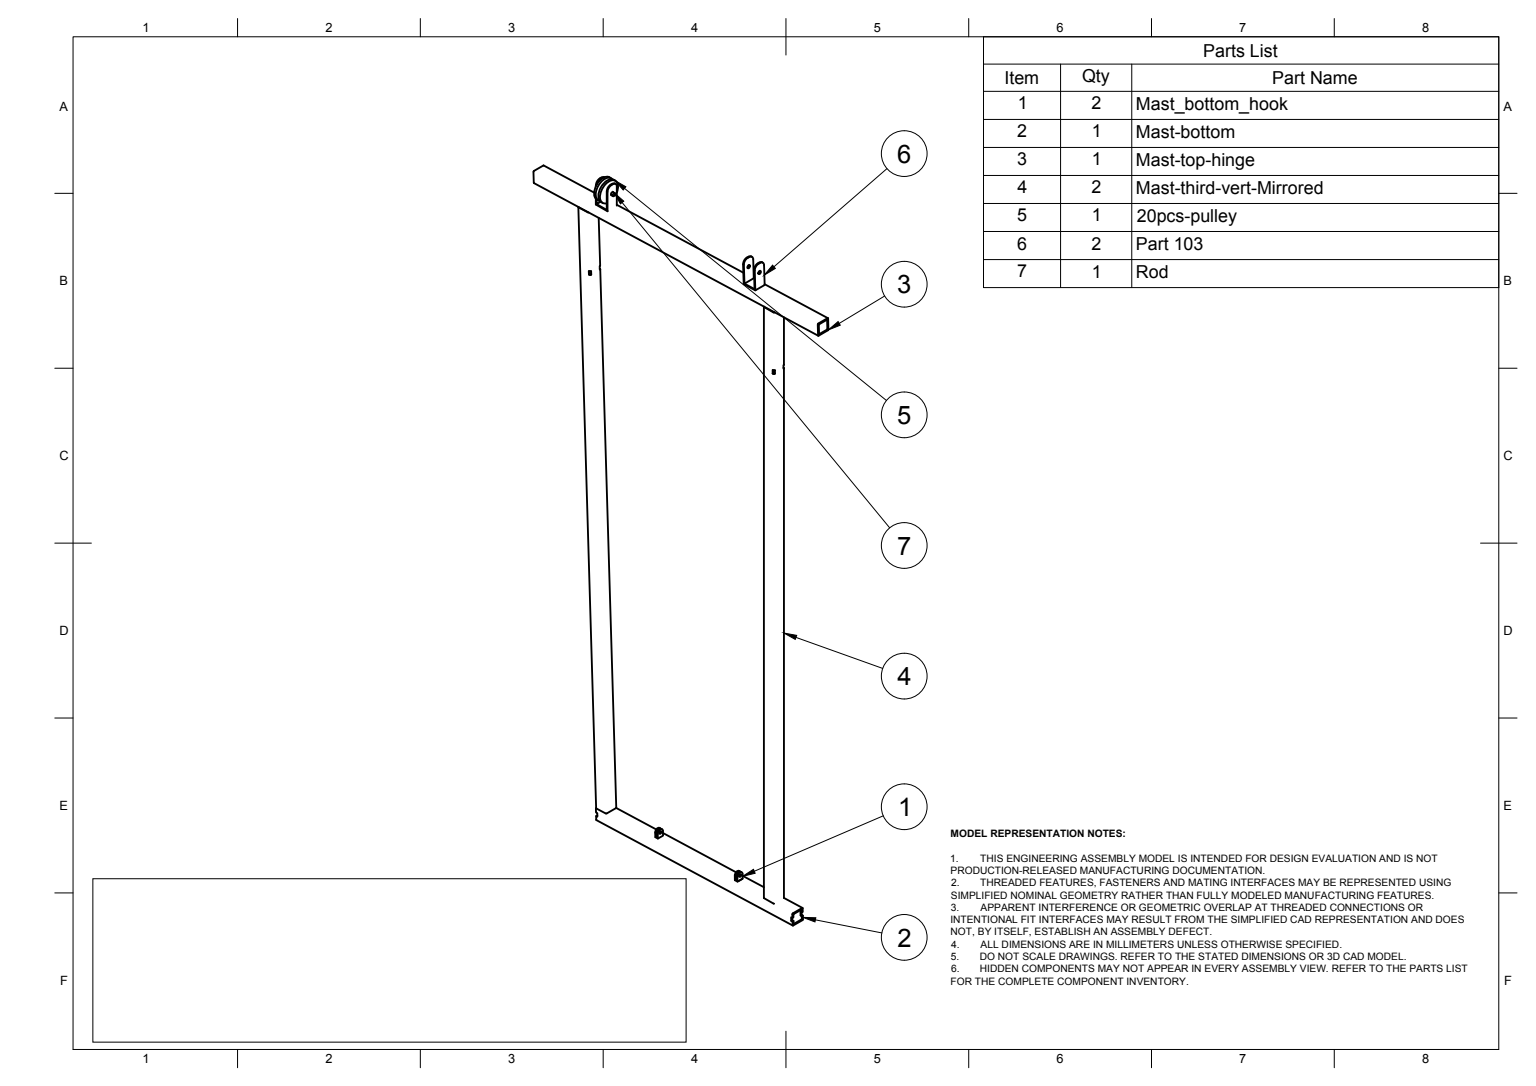
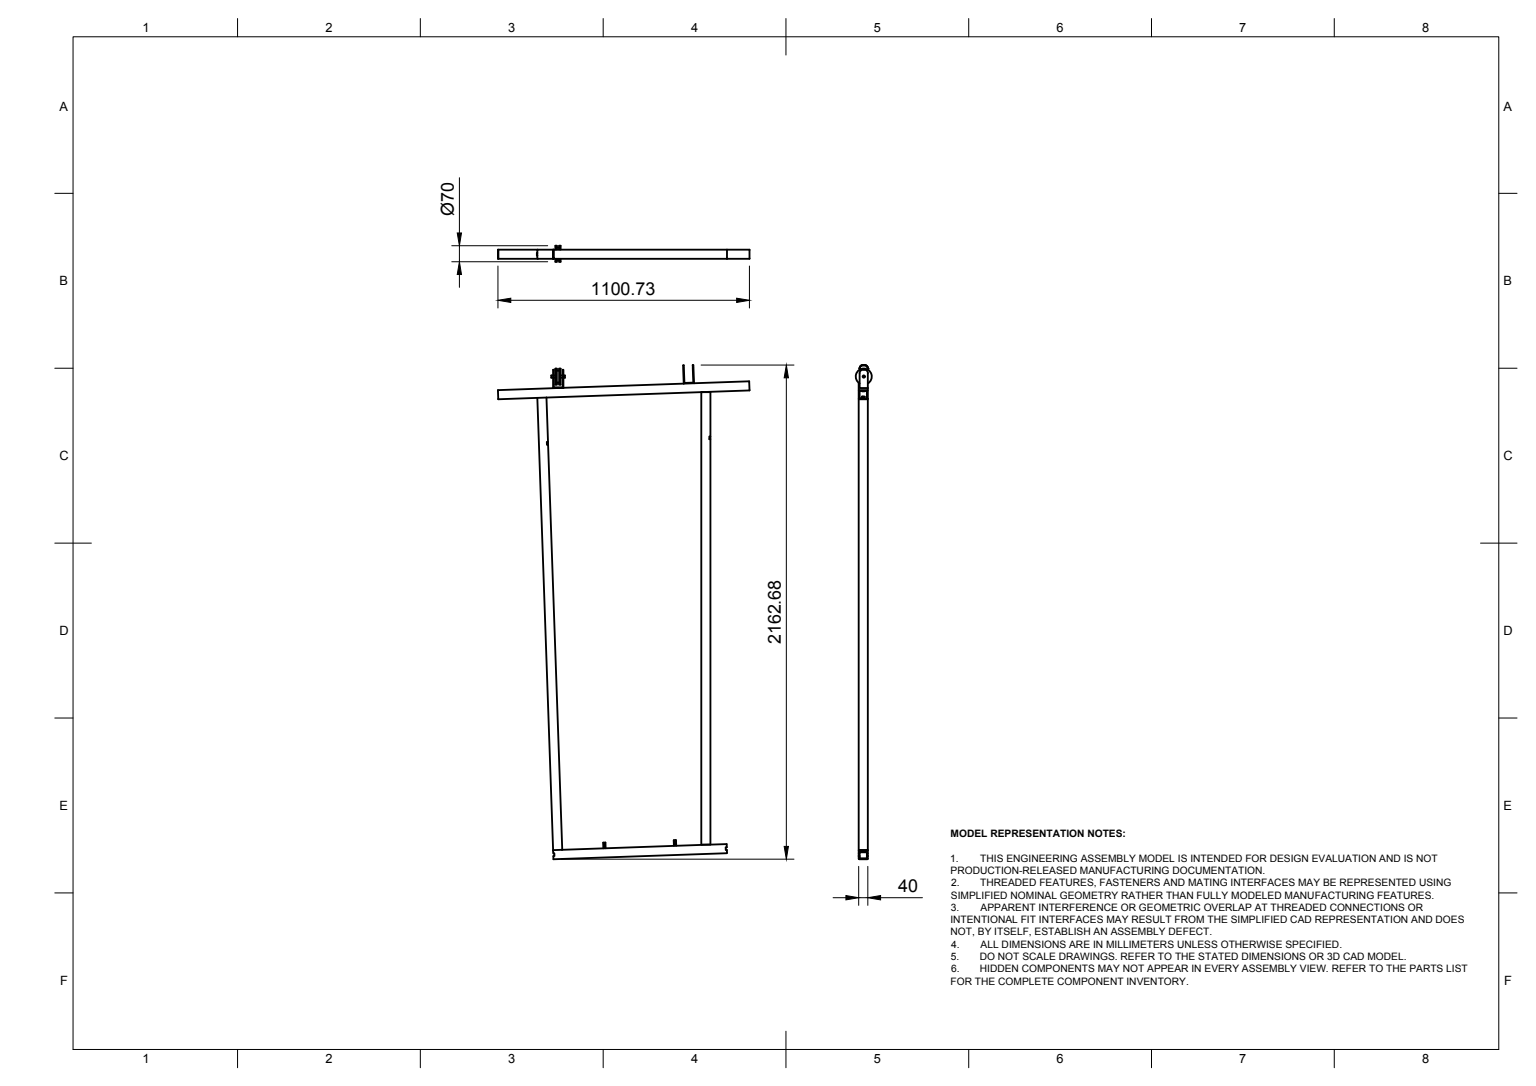
ISO-10303-21;
HEADER;
/* Generated by software containing ST-Developer
 * from STEP Tools, Inc. (www.steptools.com) 
 */

FILE_DESCRIPTION(
/* description */ (''),
/* implementation_level */ '2;1');

FILE_NAME(
/* name */ 'MAS-605',
/* time_stamp */ '2026-10-07T11:02:43-07:00',
/* author */ (''),
/* organization */ (''),
/* preprocessor_version */ 'ST-DEVELOPER v20.2',
/* originating_system */ 'Autodesk Translation Framework v15.15.0.0',
/* authorisation */ '');

FILE_SCHEMA (('AUTOMOTIVE_DESIGN { 1 0 10303 214 3 1 1 }'));
ENDSEC;

DATA;
#10=MECHANICAL_DESIGN_GEOMETRIC_PRESENTATION_REPRESENTATION('',(#66,#67,
#68,#69,#70,#71,#72),#5505);
#11=ITEM_DEFINED_TRANSFORMATION($,$,#3575,#3635);
#12=ITEM_DEFINED_TRANSFORMATION($,$,#3379,#3636);
#13=ITEM_DEFINED_TRANSFORMATION($,$,#3436,#3637);
#14=ITEM_DEFINED_TRANSFORMATION($,$,#3519,#3638);
#15=ITEM_DEFINED_TRANSFORMATION($,$,#3495,#3639);
#16=ITEM_DEFINED_TRANSFORMATION($,$,#3601,#3640);
#17=ITEM_DEFINED_TRANSFORMATION($,$,#3513,#3641);
#18=ITEM_DEFINED_TRANSFORMATION($,$,#3519,#3642);
#19=ITEM_DEFINED_TRANSFORMATION($,$,#3575,#3643);
#20=ITEM_DEFINED_TRANSFORMATION($,$,#3601,#3644);
#21=(
REPRESENTATION_RELATIONSHIP($,$,#5542,#5536)
REPRESENTATION_RELATIONSHIP_WITH_TRANSFORMATION(#11)
SHAPE_REPRESENTATION_RELATIONSHIP()
);
#22=(
REPRESENTATION_RELATIONSHIP($,$,#5537,#5536)
REPRESENTATION_RELATIONSHIP_WITH_TRANSFORMATION(#12)
SHAPE_REPRESENTATION_RELATIONSHIP()
);
#23=(
REPRESENTATION_RELATIONSHIP($,$,#5538,#5536)
REPRESENTATION_RELATIONSHIP_WITH_TRANSFORMATION(#13)
SHAPE_REPRESENTATION_RELATIONSHIP()
);
#24=(
REPRESENTATION_RELATIONSHIP($,$,#5541,#5536)
REPRESENTATION_RELATIONSHIP_WITH_TRANSFORMATION(#14)
SHAPE_REPRESENTATION_RELATIONSHIP()
);
#25=(
REPRESENTATION_RELATIONSHIP($,$,#5539,#5536)
REPRESENTATION_RELATIONSHIP_WITH_TRANSFORMATION(#15)
SHAPE_REPRESENTATION_RELATIONSHIP()
);
#26=(
REPRESENTATION_RELATIONSHIP($,$,#5543,#5536)
REPRESENTATION_RELATIONSHIP_WITH_TRANSFORMATION(#16)
SHAPE_REPRESENTATION_RELATIONSHIP()
);
#27=(
REPRESENTATION_RELATIONSHIP($,$,#5540,#5536)
REPRESENTATION_RELATIONSHIP_WITH_TRANSFORMATION(#17)
SHAPE_REPRESENTATION_RELATIONSHIP()
);
#28=(
REPRESENTATION_RELATIONSHIP($,$,#5541,#5536)
REPRESENTATION_RELATIONSHIP_WITH_TRANSFORMATION(#18)
SHAPE_REPRESENTATION_RELATIONSHIP()
);
#29=(
REPRESENTATION_RELATIONSHIP($,$,#5542,#5536)
REPRESENTATION_RELATIONSHIP_WITH_TRANSFORMATION(#19)
SHAPE_REPRESENTATION_RELATIONSHIP()
);
#30=(
REPRESENTATION_RELATIONSHIP($,$,#5543,#5536)
REPRESENTATION_RELATIONSHIP_WITH_TRANSFORMATION(#20)
SHAPE_REPRESENTATION_RELATIONSHIP()
);
#31=CONTEXT_DEPENDENT_SHAPE_REPRESENTATION(#21,#5526);
#32=CONTEXT_DEPENDENT_SHAPE_REPRESENTATION(#22,#5527);
#33=CONTEXT_DEPENDENT_SHAPE_REPRESENTATION(#23,#5528);
#34=CONTEXT_DEPENDENT_SHAPE_REPRESENTATION(#24,#5529);
#35=CONTEXT_DEPENDENT_SHAPE_REPRESENTATION(#25,#5530);
#36=CONTEXT_DEPENDENT_SHAPE_REPRESENTATION(#26,#5531);
#37=CONTEXT_DEPENDENT_SHAPE_REPRESENTATION(#27,#5532);
#38=CONTEXT_DEPENDENT_SHAPE_REPRESENTATION(#28,#5533);
#39=CONTEXT_DEPENDENT_SHAPE_REPRESENTATION(#29,#5534);
#40=CONTEXT_DEPENDENT_SHAPE_REPRESENTATION(#30,#5535);
#41=NEXT_ASSEMBLY_USAGE_OCCURRENCE('Mast_bottom_hook:1',
'Mast_bottom_hook:1','Mast_bottom_hook:1',#5545,#5551,
'Mast_bottom_hook:1');
#42=NEXT_ASSEMBLY_USAGE_OCCURRENCE('Mast-bottom:1','Mast-bottom:1',
'Mast-bottom:1',#5545,#5546,'Mast-bottom:1');
#43=NEXT_ASSEMBLY_USAGE_OCCURRENCE('Mast-top-hinge:1',
'Mast-top-hinge:1','Mast-top-hinge:1',#5545,#5547,'Mast-top-hinge:1');
#44=NEXT_ASSEMBLY_USAGE_OCCURRENCE('Mast-third-vert-Mirrored:1',
'Mast-third-vert-Mirrored:1','Mast-third-vert-Mirrored:1',#5545,#5550,
'Mast-third-vert-Mirrored:1');
#45=NEXT_ASSEMBLY_USAGE_OCCURRENCE('Pulley:1','Pulley:1','Pulley:1',#5545,
#5548,'Pulley:1');
#46=NEXT_ASSEMBLY_USAGE_OCCURRENCE('Part 103:1','Part 103:1',
'Part 103:1',#5545,#5552,'Part 103:1');
#47=NEXT_ASSEMBLY_USAGE_OCCURRENCE('rod:1','rod:1','rod:1',#5545,#5549,
'rod:1');
#48=NEXT_ASSEMBLY_USAGE_OCCURRENCE('Mast-third-vert-Mirrored:2',
'Mast-third-vert-Mirrored:2','Mast-third-vert-Mirrored:2',#5545,#5550,
'Mast-third-vert-Mirrored:2');
#49=NEXT_ASSEMBLY_USAGE_OCCURRENCE('Mast_bottom_hook:2',
'Mast_bottom_hook:2','Mast_bottom_hook:2',#5545,#5551,
'Mast_bottom_hook:2');
#50=NEXT_ASSEMBLY_USAGE_OCCURRENCE('Part 103:2','Part 103:2',
'Part 103:2',#5545,#5552,'Part 103:2');
#51=TOROIDAL_SURFACE('',#3505,30.,5.);
#52=SHAPE_REPRESENTATION_RELATIONSHIP('SRR','None',#5537,#59);
#53=SHAPE_REPRESENTATION_RELATIONSHIP('SRR','None',#5538,#60);
#54=SHAPE_REPRESENTATION_RELATIONSHIP('SRR','None',#5539,#61);
#55=SHAPE_REPRESENTATION_RELATIONSHIP('SRR','None',#5540,#62);
#56=SHAPE_REPRESENTATION_RELATIONSHIP('SRR','None',#5541,#63);
#57=SHAPE_REPRESENTATION_RELATIONSHIP('SRR','None',#5542,#64);
#58=SHAPE_REPRESENTATION_RELATIONSHIP('SRR','None',#5543,#65);
#59=ADVANCED_BREP_SHAPE_REPRESENTATION('',(#73),#5498);
#60=ADVANCED_BREP_SHAPE_REPRESENTATION('',(#74),#5499);
#61=ADVANCED_BREP_SHAPE_REPRESENTATION('',(#75),#5500);
#62=ADVANCED_BREP_SHAPE_REPRESENTATION('',(#76),#5501);
#63=ADVANCED_BREP_SHAPE_REPRESENTATION('',(#77),#5502);
#64=ADVANCED_BREP_SHAPE_REPRESENTATION('',(#78),#5503);
#65=ADVANCED_BREP_SHAPE_REPRESENTATION('',(#79),#5504);
#66=STYLED_ITEM('',(#5581),#73);
#67=STYLED_ITEM('',(#5582),#74);
#68=STYLED_ITEM('',(#5583),#75);
#69=STYLED_ITEM('',(#5584),#76);
#70=STYLED_ITEM('',(#5585),#77);
#71=STYLED_ITEM('',(#5586),#78);
#72=STYLED_ITEM('',(#5587),#79);
#73=MANIFOLD_SOLID_BREP('Body1',#3293);
#74=MANIFOLD_SOLID_BREP('Body1',#3294);
#75=MANIFOLD_SOLID_BREP('Body1',#3295);
#76=MANIFOLD_SOLID_BREP('Body1',#3296);
#77=MANIFOLD_SOLID_BREP('Body1',#3297);
#78=MANIFOLD_SOLID_BREP('Body1',#3298);
#79=MANIFOLD_SOLID_BREP('Body1',#3299);
#80=FACE_BOUND('',#416,.T.);
#81=FACE_BOUND('',#417,.T.);
#82=FACE_BOUND('',#428,.T.);
#83=FACE_BOUND('',#429,.T.);
#84=FACE_BOUND('',#447,.T.);
#85=FACE_BOUND('',#448,.T.);
#86=FACE_BOUND('',#450,.T.);
#87=FACE_BOUND('',#451,.T.);
#88=FACE_BOUND('',#461,.T.);
#89=FACE_BOUND('',#462,.T.);
#90=FACE_BOUND('',#463,.T.);
#91=FACE_BOUND('',#464,.T.);
#92=FACE_BOUND('',#466,.T.);
#93=FACE_BOUND('',#467,.T.);
#94=FACE_BOUND('',#468,.T.);
#95=FACE_BOUND('',#469,.T.);
#96=FACE_BOUND('',#477,.T.);
#97=FACE_BOUND('',#479,.T.);
#98=FACE_BOUND('',#504,.T.);
#99=FACE_BOUND('',#507,.T.);
#100=FACE_BOUND('',#510,.T.);
#101=FACE_BOUND('',#513,.T.);
#102=FACE_BOUND('',#532,.T.);
#103=FACE_BOUND('',#554,.T.);
#104=FACE_BOUND('',#556,.T.);
#105=FACE_BOUND('',#558,.T.);
#106=FACE_BOUND('',#560,.T.);
#107=FACE_BOUND('',#562,.T.);
#108=FACE_BOUND('',#577,.T.);
#109=FACE_BOUND('',#579,.T.);
#110=FACE_BOUND('',#582,.T.);
#111=FACE_BOUND('',#584,.T.);
#112=FACE_BOUND('',#586,.T.);
#113=CYLINDRICAL_SURFACE('',#3399,2.);
#114=CYLINDRICAL_SURFACE('',#3401,2.);
#115=CYLINDRICAL_SURFACE('',#3404,2.);
#116=CYLINDRICAL_SURFACE('',#3406,2.);
#117=CYLINDRICAL_SURFACE('',#3414,1.8);
#118=CYLINDRICAL_SURFACE('',#3415,1.8);
#119=CYLINDRICAL_SURFACE('',#3417,1.8);
#120=CYLINDRICAL_SURFACE('',#3418,1.8);
#121=CYLINDRICAL_SURFACE('',#3450,2.);
#122=CYLINDRICAL_SURFACE('',#3453,2.);
#123=CYLINDRICAL_SURFACE('',#3457,2.);
#124=CYLINDRICAL_SURFACE('',#3460,2.);
#125=CYLINDRICAL_SURFACE('',#3473,1.8);
#126=CYLINDRICAL_SURFACE('',#3474,1.8);
#127=CYLINDRICAL_SURFACE('',#3476,1.8);
#128=CYLINDRICAL_SURFACE('',#3477,1.8);
#129=CYLINDRICAL_SURFACE('',#3496,5.);
#130=CYLINDRICAL_SURFACE('',#3501,35.);
#131=CYLINDRICAL_SURFACE('',#3510,35.);
#132=CYLINDRICAL_SURFACE('',#3516,5.);
#133=CYLINDRICAL_SURFACE('',#3531,2.);
#134=CYLINDRICAL_SURFACE('',#3535,2.);
#135=CYLINDRICAL_SURFACE('',#3538,1.8);
#136=CYLINDRICAL_SURFACE('',#3541,1.8);
#137=CYLINDRICAL_SURFACE('',#3544,1.8);
#138=CYLINDRICAL_SURFACE('',#3547,1.8);
#139=CYLINDRICAL_SURFACE('',#3553,2.);
#140=CYLINDRICAL_SURFACE('',#3556,2.);
#141=CYLINDRICAL_SURFACE('',#3558,2.);
#142=CYLINDRICAL_SURFACE('',#3559,2.);
#143=CYLINDRICAL_SURFACE('',#3592,4.);
#144=CYLINDRICAL_SURFACE('',#3593,4.);
#145=CYLINDRICAL_SURFACE('',#3594,10.);
#146=CYLINDRICAL_SURFACE('',#3595,10.);
#147=CYLINDRICAL_SURFACE('',#3629,15.);
#148=CYLINDRICAL_SURFACE('',#3630,15.);
#149=CYLINDRICAL_SURFACE('',#3631,15.);
#150=CYLINDRICAL_SURFACE('',#3632,15.);
#151=CYLINDRICAL_SURFACE('',#3633,5.);
#152=CYLINDRICAL_SURFACE('',#3634,5.);
#153=CIRCLE('',#3385,1.8);
#154=CIRCLE('',#3386,1.8);
#155=CIRCLE('',#3387,2.);
#156=CIRCLE('',#3388,2.);
#157=CIRCLE('',#3392,2.);
#158=CIRCLE('',#3393,2.);
#159=CIRCLE('',#3394,1.8);
#160=CIRCLE('',#3395,1.8);
#161=CIRCLE('',#3400,2.);
#162=CIRCLE('',#3402,2.);
#163=CIRCLE('',#3405,2.);
#164=CIRCLE('',#3407,2.);
#165=CIRCLE('',#3409,1.8);
#166=CIRCLE('',#3410,1.8);
#167=CIRCLE('',#3412,1.8);
#168=CIRCLE('',#3413,1.8);
#169=CIRCLE('',#3451,2.);
#170=CIRCLE('',#3452,2.);
#171=CIRCLE('',#3454,2.);
#172=CIRCLE('',#3455,2.);
#173=CIRCLE('',#3458,2.);
#174=CIRCLE('',#3459,2.);
#175=CIRCLE('',#3461,2.);
#176=CIRCLE('',#3462,2.);
#177=CIRCLE('',#3464,1.8);
#178=CIRCLE('',#3465,1.8);
#179=CIRCLE('',#3466,1.8);
#180=CIRCLE('',#3467,1.8);
#181=CIRCLE('',#3469,1.8);
#182=CIRCLE('',#3470,1.8);
#183=CIRCLE('',#3471,1.8);
#184=CIRCLE('',#3472,1.8);
#185=CIRCLE('',#3497,5.);
#186=CIRCLE('',#3498,5.);
#187=CIRCLE('',#3500,35.);
#188=CIRCLE('',#3502,35.);
#189=CIRCLE('',#3504,30.);
#190=CIRCLE('',#3506,5.);
#191=CIRCLE('',#3507,30.);
#192=CIRCLE('',#3509,35.);
#193=CIRCLE('',#3511,35.);
#194=CIRCLE('',#3515,5.);
#195=CIRCLE('',#3517,5.);
#196=CIRCLE('',#3521,1.8);
#197=CIRCLE('',#3522,1.8);
#198=CIRCLE('',#3523,2.);
#199=CIRCLE('',#3524,2.);
#200=CIRCLE('',#3526,2.);
#201=CIRCLE('',#3527,2.);
#202=CIRCLE('',#3528,1.8);
#203=CIRCLE('',#3529,1.8);
#204=CIRCLE('',#3532,2.);
#205=CIRCLE('',#3533,2.);
#206=CIRCLE('',#3536,2.);
#207=CIRCLE('',#3539,1.8);
#208=CIRCLE('',#3542,1.8);
#209=CIRCLE('',#3545,1.8);
#210=CIRCLE('',#3548,1.8);
#211=CIRCLE('',#3550,2.);
#212=CIRCLE('',#3551,2.);
#213=CIRCLE('',#3552,2.);
#214=CIRCLE('',#3554,2.);
#215=CIRCLE('',#3560,2.);
#216=CIRCLE('',#3578,10.);
#217=CIRCLE('',#3579,4.);
#218=CIRCLE('',#3581,10.);
#219=CIRCLE('',#3582,4.);
#220=CIRCLE('',#3584,10.);
#221=CIRCLE('',#3585,4.);
#222=CIRCLE('',#3587,10.);
#223=CIRCLE('',#3588,4.);
#224=CIRCLE('',#3604,15.);
#225=CIRCLE('',#3605,15.);
#226=CIRCLE('',#3606,5.);
#227=CIRCLE('',#3608,15.);
#228=CIRCLE('',#3609,15.);
#229=CIRCLE('',#3610,5.);
#230=CIRCLE('',#3613,15.);
#231=CIRCLE('',#3614,15.);
#232=CIRCLE('',#3615,5.);
#233=CIRCLE('',#3617,15.);
#234=CIRCLE('',#3618,15.);
#235=CIRCLE('',#3619,5.);
#236=FACE_OUTER_BOUND('',#402,.T.);
#237=FACE_OUTER_BOUND('',#403,.T.);
#238=FACE_OUTER_BOUND('',#404,.T.);
#239=FACE_OUTER_BOUND('',#405,.T.);
#240=FACE_OUTER_BOUND('',#406,.T.);
#241=FACE_OUTER_BOUND('',#407,.T.);
#242=FACE_OUTER_BOUND('',#408,.T.);
#243=FACE_OUTER_BOUND('',#409,.T.);
#244=FACE_OUTER_BOUND('',#410,.T.);
#245=FACE_OUTER_BOUND('',#411,.T.);
#246=FACE_OUTER_BOUND('',#412,.T.);
#247=FACE_OUTER_BOUND('',#413,.T.);
#248=FACE_OUTER_BOUND('',#414,.T.);
#249=FACE_OUTER_BOUND('',#415,.T.);
#250=FACE_OUTER_BOUND('',#418,.T.);
#251=FACE_OUTER_BOUND('',#419,.T.);
#252=FACE_OUTER_BOUND('',#420,.T.);
#253=FACE_OUTER_BOUND('',#421,.T.);
#254=FACE_OUTER_BOUND('',#422,.T.);
#255=FACE_OUTER_BOUND('',#423,.T.);
#256=FACE_OUTER_BOUND('',#424,.T.);
#257=FACE_OUTER_BOUND('',#425,.T.);
#258=FACE_OUTER_BOUND('',#426,.T.);
#259=FACE_OUTER_BOUND('',#427,.T.);
#260=FACE_OUTER_BOUND('',#430,.T.);
#261=FACE_OUTER_BOUND('',#431,.T.);
#262=FACE_OUTER_BOUND('',#432,.T.);
#263=FACE_OUTER_BOUND('',#433,.T.);
#264=FACE_OUTER_BOUND('',#434,.T.);
#265=FACE_OUTER_BOUND('',#435,.T.);
#266=FACE_OUTER_BOUND('',#436,.T.);
#267=FACE_OUTER_BOUND('',#437,.T.);
#268=FACE_OUTER_BOUND('',#438,.T.);
#269=FACE_OUTER_BOUND('',#439,.T.);
#270=FACE_OUTER_BOUND('',#440,.T.);
#271=FACE_OUTER_BOUND('',#441,.T.);
#272=FACE_OUTER_BOUND('',#442,.T.);
#273=FACE_OUTER_BOUND('',#443,.T.);
#274=FACE_OUTER_BOUND('',#444,.T.);
#275=FACE_OUTER_BOUND('',#445,.T.);
#276=FACE_OUTER_BOUND('',#446,.T.);
#277=FACE_OUTER_BOUND('',#449,.T.);
#278=FACE_OUTER_BOUND('',#452,.T.);
#279=FACE_OUTER_BOUND('',#453,.T.);
#280=FACE_OUTER_BOUND('',#454,.T.);
#281=FACE_OUTER_BOUND('',#455,.T.);
#282=FACE_OUTER_BOUND('',#456,.T.);
#283=FACE_OUTER_BOUND('',#457,.T.);
#284=FACE_OUTER_BOUND('',#458,.T.);
#285=FACE_OUTER_BOUND('',#459,.T.);
#286=FACE_OUTER_BOUND('',#460,.T.);
#287=FACE_OUTER_BOUND('',#465,.T.);
#288=FACE_OUTER_BOUND('',#470,.T.);
#289=FACE_OUTER_BOUND('',#471,.T.);
#290=FACE_OUTER_BOUND('',#472,.T.);
#291=FACE_OUTER_BOUND('',#473,.T.);
#292=FACE_OUTER_BOUND('',#474,.T.);
#293=FACE_OUTER_BOUND('',#475,.T.);
#294=FACE_OUTER_BOUND('',#476,.T.);
#295=FACE_OUTER_BOUND('',#478,.T.);
#296=FACE_OUTER_BOUND('',#480,.T.);
#297=FACE_OUTER_BOUND('',#481,.T.);
#298=FACE_OUTER_BOUND('',#482,.T.);
#299=FACE_OUTER_BOUND('',#483,.T.);
#300=FACE_OUTER_BOUND('',#484,.T.);
#301=FACE_OUTER_BOUND('',#485,.T.);
#302=FACE_OUTER_BOUND('',#486,.T.);
#303=FACE_OUTER_BOUND('',#487,.T.);
#304=FACE_OUTER_BOUND('',#488,.T.);
#305=FACE_OUTER_BOUND('',#489,.T.);
#306=FACE_OUTER_BOUND('',#490,.T.);
#307=FACE_OUTER_BOUND('',#491,.T.);
#308=FACE_OUTER_BOUND('',#492,.T.);
#309=FACE_OUTER_BOUND('',#493,.T.);
#310=FACE_OUTER_BOUND('',#494,.T.);
#311=FACE_OUTER_BOUND('',#495,.T.);
#312=FACE_OUTER_BOUND('',#496,.T.);
#313=FACE_OUTER_BOUND('',#497,.T.);
#314=FACE_OUTER_BOUND('',#498,.T.);
#315=FACE_OUTER_BOUND('',#499,.T.);
#316=FACE_OUTER_BOUND('',#500,.T.);
#317=FACE_OUTER_BOUND('',#501,.T.);
#318=FACE_OUTER_BOUND('',#502,.T.);
#319=FACE_OUTER_BOUND('',#503,.T.);
#320=FACE_OUTER_BOUND('',#505,.T.);
#321=FACE_OUTER_BOUND('',#506,.T.);
#322=FACE_OUTER_BOUND('',#508,.T.);
#323=FACE_OUTER_BOUND('',#509,.T.);
#324=FACE_OUTER_BOUND('',#511,.T.);
#325=FACE_OUTER_BOUND('',#512,.T.);
#326=FACE_OUTER_BOUND('',#514,.T.);
#327=FACE_OUTER_BOUND('',#515,.T.);
#328=FACE_OUTER_BOUND('',#516,.T.);
#329=FACE_OUTER_BOUND('',#517,.T.);
#330=FACE_OUTER_BOUND('',#518,.T.);
#331=FACE_OUTER_BOUND('',#519,.T.);
#332=FACE_OUTER_BOUND('',#520,.T.);
#333=FACE_OUTER_BOUND('',#521,.T.);
#334=FACE_OUTER_BOUND('',#522,.T.);
#335=FACE_OUTER_BOUND('',#523,.T.);
#336=FACE_OUTER_BOUND('',#524,.T.);
#337=FACE_OUTER_BOUND('',#525,.T.);
#338=FACE_OUTER_BOUND('',#526,.T.);
#339=FACE_OUTER_BOUND('',#527,.T.);
#340=FACE_OUTER_BOUND('',#528,.T.);
#341=FACE_OUTER_BOUND('',#529,.T.);
#342=FACE_OUTER_BOUND('',#530,.T.);
#343=FACE_OUTER_BOUND('',#531,.T.);
#344=FACE_OUTER_BOUND('',#533,.T.);
#345=FACE_OUTER_BOUND('',#534,.T.);
#346=FACE_OUTER_BOUND('',#535,.T.);
#347=FACE_OUTER_BOUND('',#536,.T.);
#348=FACE_OUTER_BOUND('',#537,.T.);
#349=FACE_OUTER_BOUND('',#538,.T.);
#350=FACE_OUTER_BOUND('',#539,.T.);
#351=FACE_OUTER_BOUND('',#540,.T.);
#352=FACE_OUTER_BOUND('',#541,.T.);
#353=FACE_OUTER_BOUND('',#542,.T.);
#354=FACE_OUTER_BOUND('',#543,.T.);
#355=FACE_OUTER_BOUND('',#544,.T.);
#356=FACE_OUTER_BOUND('',#545,.T.);
#357=FACE_OUTER_BOUND('',#546,.T.);
#358=FACE_OUTER_BOUND('',#547,.T.);
#359=FACE_OUTER_BOUND('',#548,.T.);
#360=FACE_OUTER_BOUND('',#549,.T.);
#361=FACE_OUTER_BOUND('',#550,.T.);
#362=FACE_OUTER_BOUND('',#551,.T.);
#363=FACE_OUTER_BOUND('',#552,.T.);
#364=FACE_OUTER_BOUND('',#553,.T.);
#365=FACE_OUTER_BOUND('',#555,.T.);
#366=FACE_OUTER_BOUND('',#557,.T.);
#367=FACE_OUTER_BOUND('',#559,.T.);
#368=FACE_OUTER_BOUND('',#561,.T.);
#369=FACE_OUTER_BOUND('',#563,.T.);
#370=FACE_OUTER_BOUND('',#564,.T.);
#371=FACE_OUTER_BOUND('',#565,.T.);
#372=FACE_OUTER_BOUND('',#566,.T.);
#373=FACE_OUTER_BOUND('',#567,.T.);
#374=FACE_OUTER_BOUND('',#568,.T.);
#375=FACE_OUTER_BOUND('',#569,.T.);
#376=FACE_OUTER_BOUND('',#570,.T.);
#377=FACE_OUTER_BOUND('',#571,.T.);
#378=FACE_OUTER_BOUND('',#572,.T.);
#379=FACE_OUTER_BOUND('',#573,.T.);
#380=FACE_OUTER_BOUND('',#574,.T.);
#381=FACE_OUTER_BOUND('',#575,.T.);
#382=FACE_OUTER_BOUND('',#576,.T.);
#383=FACE_OUTER_BOUND('',#578,.T.);
#384=FACE_OUTER_BOUND('',#580,.T.);
#385=FACE_OUTER_BOUND('',#581,.T.);
#386=FACE_OUTER_BOUND('',#583,.T.);
#387=FACE_OUTER_BOUND('',#585,.T.);
#388=FACE_OUTER_BOUND('',#587,.T.);
#389=FACE_OUTER_BOUND('',#588,.T.);
#390=FACE_OUTER_BOUND('',#589,.T.);
#391=FACE_OUTER_BOUND('',#590,.T.);
#392=FACE_OUTER_BOUND('',#591,.T.);
#393=FACE_OUTER_BOUND('',#592,.T.);
#394=FACE_OUTER_BOUND('',#593,.T.);
#395=FACE_OUTER_BOUND('',#594,.T.);
#396=FACE_OUTER_BOUND('',#595,.T.);
#397=FACE_OUTER_BOUND('',#596,.T.);
#398=FACE_OUTER_BOUND('',#597,.T.);
#399=FACE_OUTER_BOUND('',#598,.T.);
#400=FACE_OUTER_BOUND('',#599,.T.);
#401=FACE_OUTER_BOUND('',#600,.T.);
#402=EDGE_LOOP('',(#2096,#2097,#2098,#2099));
#403=EDGE_LOOP('',(#2100,#2101,#2102,#2103));
#404=EDGE_LOOP('',(#2104,#2105,#2106,#2107));
#405=EDGE_LOOP('',(#2108,#2109,#2110,#2111));
#406=EDGE_LOOP('',(#2112,#2113,#2114,#2115,#2116,#2117,#2118,#2119,#2120,
#2121,#2122,#2123));
#407=EDGE_LOOP('',(#2124,#2125,#2126,#2127,#2128,#2129,#2130,#2131,#2132,
#2133,#2134,#2135));
#408=EDGE_LOOP('',(#2136,#2137,#2138,#2139,#2140,#2141,#2142,#2143,#2144,
#2145,#2146,#2147));
#409=EDGE_LOOP('',(#2148,#2149,#2150,#2151,#2152,#2153,#2154,#2155,#2156,
#2157,#2158,#2159));
#410=EDGE_LOOP('',(#2160,#2161,#2162,#2163,#2164,#2165,#2166,#2167,#2168,
#2169,#2170,#2171));
#411=EDGE_LOOP('',(#2172,#2173,#2174,#2175,#2176,#2177,#2178,#2179,#2180,
#2181,#2182,#2183));
#412=EDGE_LOOP('',(#2184,#2185,#2186,#2187));
#413=EDGE_LOOP('',(#2188,#2189,#2190,#2191));
#414=EDGE_LOOP('',(#2192,#2193,#2194,#2195));
#415=EDGE_LOOP('',(#2196,#2197,#2198,#2199));
#416=EDGE_LOOP('',(#2200,#2201,#2202,#2203));
#417=EDGE_LOOP('',(#2204,#2205,#2206,#2207));
#418=EDGE_LOOP('',(#2208,#2209,#2210,#2211));
#419=EDGE_LOOP('',(#2212,#2213,#2214,#2215));
#420=EDGE_LOOP('',(#2216,#2217,#2218,#2219,#2220,#2221,#2222,#2223,#2224,
#2225,#2226,#2227));
#421=EDGE_LOOP('',(#2228,#2229,#2230,#2231,#2232,#2233,#2234,#2235,#2236,
#2237,#2238,#2239));
#422=EDGE_LOOP('',(#2240,#2241,#2242,#2243));
#423=EDGE_LOOP('',(#2244,#2245,#2246,#2247));
#424=EDGE_LOOP('',(#2248,#2249,#2250,#2251));
#425=EDGE_LOOP('',(#2252,#2253,#2254,#2255));
#426=EDGE_LOOP('',(#2256,#2257,#2258,#2259));
#427=EDGE_LOOP('',(#2260,#2261,#2262,#2263));
#428=EDGE_LOOP('',(#2264,#2265,#2266,#2267));
#429=EDGE_LOOP('',(#2268,#2269,#2270,#2271));
#430=EDGE_LOOP('',(#2272,#2273,#2274,#2275));
#431=EDGE_LOOP('',(#2276,#2277,#2278,#2279));
#432=EDGE_LOOP('',(#2280,#2281,#2282,#2283));
#433=EDGE_LOOP('',(#2284,#2285,#2286,#2287));
#434=EDGE_LOOP('',(#2288,#2289,#2290,#2291));
#435=EDGE_LOOP('',(#2292,#2293,#2294,#2295));
#436=EDGE_LOOP('',(#2296,#2297,#2298,#2299));
#437=EDGE_LOOP('',(#2300,#2301,#2302,#2303));
#438=EDGE_LOOP('',(#2304,#2305,#2306,#2307));
#439=EDGE_LOOP('',(#2308,#2309,#2310,#2311));
#440=EDGE_LOOP('',(#2312,#2313,#2314,#2315));
#441=EDGE_LOOP('',(#2316,#2317,#2318,#2319));
#442=EDGE_LOOP('',(#2320,#2321,#2322,#2323));
#443=EDGE_LOOP('',(#2324,#2325,#2326,#2327));
#444=EDGE_LOOP('',(#2328,#2329,#2330,#2331));
#445=EDGE_LOOP('',(#2332,#2333,#2334,#2335));
#446=EDGE_LOOP('',(#2336,#2337,#2338,#2339));
#447=EDGE_LOOP('',(#2340,#2341,#2342,#2343));
#448=EDGE_LOOP('',(#2344,#2345,#2346,#2347));
#449=EDGE_LOOP('',(#2348,#2349,#2350,#2351));
#450=EDGE_LOOP('',(#2352,#2353,#2354,#2355));
#451=EDGE_LOOP('',(#2356,#2357,#2358,#2359));
#452=EDGE_LOOP('',(#2360,#2361,#2362,#2363));
#453=EDGE_LOOP('',(#2364,#2365,#2366,#2367));
#454=EDGE_LOOP('',(#2368,#2369,#2370,#2371));
#455=EDGE_LOOP('',(#2372,#2373,#2374,#2375));
#456=EDGE_LOOP('',(#2376,#2377,#2378,#2379));
#457=EDGE_LOOP('',(#2380,#2381,#2382,#2383));
#458=EDGE_LOOP('',(#2384,#2385,#2386,#2387));
#459=EDGE_LOOP('',(#2388,#2389,#2390,#2391));
#460=EDGE_LOOP('',(#2392,#2393,#2394,#2395));
#461=EDGE_LOOP('',(#2396,#2397,#2398,#2399));
#462=EDGE_LOOP('',(#2400,#2401,#2402,#2403));
#463=EDGE_LOOP('',(#2404,#2405,#2406,#2407));
#464=EDGE_LOOP('',(#2408,#2409,#2410,#2411));
#465=EDGE_LOOP('',(#2412,#2413,#2414,#2415));
#466=EDGE_LOOP('',(#2416,#2417,#2418,#2419));
#467=EDGE_LOOP('',(#2420,#2421,#2422,#2423));
#468=EDGE_LOOP('',(#2424,#2425,#2426,#2427));
#469=EDGE_LOOP('',(#2428,#2429,#2430,#2431));
#470=EDGE_LOOP('',(#2432,#2433,#2434,#2435));
#471=EDGE_LOOP('',(#2436,#2437,#2438,#2439));
#472=EDGE_LOOP('',(#2440,#2441,#2442,#2443));
#473=EDGE_LOOP('',(#2444,#2445,#2446,#2447));
#474=EDGE_LOOP('',(#2448,#2449,#2450,#2451));
#475=EDGE_LOOP('',(#2452,#2453,#2454,#2455));
#476=EDGE_LOOP('',(#2456,#2457,#2458,#2459,#2460,#2461,#2462,#2463));
#477=EDGE_LOOP('',(#2464,#2465,#2466,#2467,#2468,#2469,#2470,#2471));
#478=EDGE_LOOP('',(#2472,#2473,#2474,#2475,#2476,#2477,#2478,#2479));
#479=EDGE_LOOP('',(#2480,#2481,#2482,#2483,#2484,#2485,#2486,#2487));
#480=EDGE_LOOP('',(#2488,#2489,#2490,#2491));
#481=EDGE_LOOP('',(#2492,#2493,#2494,#2495));
#482=EDGE_LOOP('',(#2496,#2497,#2498,#2499));
#483=EDGE_LOOP('',(#2500,#2501,#2502,#2503));
#484=EDGE_LOOP('',(#2504,#2505,#2506,#2507));
#485=EDGE_LOOP('',(#2508,#2509,#2510,#2511));
#486=EDGE_LOOP('',(#2512,#2513,#2514,#2515));
#487=EDGE_LOOP('',(#2516,#2517,#2518,#2519));
#488=EDGE_LOOP('',(#2520,#2521,#2522,#2523));
#489=EDGE_LOOP('',(#2524,#2525,#2526,#2527));
#490=EDGE_LOOP('',(#2528,#2529,#2530,#2531));
#491=EDGE_LOOP('',(#2532,#2533,#2534,#2535));
#492=EDGE_LOOP('',(#2536,#2537,#2538,#2539));
#493=EDGE_LOOP('',(#2540,#2541,#2542,#2543));
#494=EDGE_LOOP('',(#2544,#2545,#2546,#2547));
#495=EDGE_LOOP('',(#2548,#2549,#2550,#2551));
#496=EDGE_LOOP('',(#2552,#2553,#2554,#2555));
#497=EDGE_LOOP('',(#2556,#2557,#2558,#2559));
#498=EDGE_LOOP('',(#2560,#2561,#2562,#2563));
#499=EDGE_LOOP('',(#2564,#2565,#2566,#2567));
#500=EDGE_LOOP('',(#2568,#2569,#2570,#2571));
#501=EDGE_LOOP('',(#2572,#2573,#2574,#2575));
#502=EDGE_LOOP('',(#2576,#2577,#2578,#2579));
#503=EDGE_LOOP('',(#2580));
#504=EDGE_LOOP('',(#2581));
#505=EDGE_LOOP('',(#2582,#2583,#2584,#2585));
#506=EDGE_LOOP('',(#2586));
#507=EDGE_LOOP('',(#2587));
#508=EDGE_LOOP('',(#2588,#2589,#2590,#2591));
#509=EDGE_LOOP('',(#2592));
#510=EDGE_LOOP('',(#2593));
#511=EDGE_LOOP('',(#2594,#2595,#2596,#2597));
#512=EDGE_LOOP('',(#2598));
#513=EDGE_LOOP('',(#2599));
#514=EDGE_LOOP('',(#2600));
#515=EDGE_LOOP('',(#2601,#2602,#2603,#2604));
#516=EDGE_LOOP('',(#2605));
#517=EDGE_LOOP('',(#2606,#2607,#2608,#2609,#2610,#2611,#2612,#2613,#2614,
#2615,#2616,#2617));
#518=EDGE_LOOP('',(#2618,#2619,#2620,#2621,#2622,#2623,#2624,#2625,#2626,
#2627,#2628,#2629));
#519=EDGE_LOOP('',(#2630,#2631,#2632,#2633,#2634,#2635,#2636,#2637));
#520=EDGE_LOOP('',(#2638,#2639,#2640,#2641));
#521=EDGE_LOOP('',(#2642,#2643,#2644,#2645,#2646,#2647,#2648,#2649,#2650,
#2651,#2652,#2653,#2654,#2655,#2656,#2657));
#522=EDGE_LOOP('',(#2658,#2659,#2660,#2661));
#523=EDGE_LOOP('',(#2662,#2663,#2664,#2665,#2666,#2667,#2668,#2669));
#524=EDGE_LOOP('',(#2670,#2671,#2672,#2673));
#525=EDGE_LOOP('',(#2674,#2675,#2676,#2677));
#526=EDGE_LOOP('',(#2678,#2679,#2680,#2681));
#527=EDGE_LOOP('',(#2682,#2683,#2684,#2685,#2686,#2687,#2688,#2689));
#528=EDGE_LOOP('',(#2690,#2691,#2692,#2693));
#529=EDGE_LOOP('',(#2694,#2695,#2696,#2697));
#530=EDGE_LOOP('',(#2698,#2699,#2700,#2701));
#531=EDGE_LOOP('',(#2702,#2703,#2704,#2705,#2706,#2707,#2708,#2709));
#532=EDGE_LOOP('',(#2710,#2711,#2712,#2713,#2714,#2715,#2716,#2717));
#533=EDGE_LOOP('',(#2718,#2719,#2720,#2721));
#534=EDGE_LOOP('',(#2722,#2723,#2724,#2725,#2726,#2727,#2728,#2729));
#535=EDGE_LOOP('',(#2730,#2731,#2732,#2733));
#536=EDGE_LOOP('',(#2734,#2735,#2736,#2737,#2738,#2739,#2740,#2741));
#537=EDGE_LOOP('',(#2742,#2743,#2744,#2745));
#538=EDGE_LOOP('',(#2746,#2747,#2748,#2749));
#539=EDGE_LOOP('',(#2750,#2751,#2752,#2753,#2754));
#540=EDGE_LOOP('',(#2755,#2756,#2757,#2758));
#541=EDGE_LOOP('',(#2759,#2760,#2761,#2762,#2763));
#542=EDGE_LOOP('',(#2764,#2765,#2766,#2767));
#543=EDGE_LOOP('',(#2768,#2769,#2770,#2771,#2772));
#544=EDGE_LOOP('',(#2773,#2774,#2775,#2776));
#545=EDGE_LOOP('',(#2777,#2778,#2779,#2780,#2781));
#546=EDGE_LOOP('',(#2782,#2783,#2784,#2785));
#547=EDGE_LOOP('',(#2786,#2787,#2788,#2789));
#548=EDGE_LOOP('',(#2790,#2791,#2792,#2793));
#549=EDGE_LOOP('',(#2794,#2795,#2796,#2797));
#550=EDGE_LOOP('',(#2798,#2799,#2800,#2801));
#551=EDGE_LOOP('',(#2802,#2803,#2804,#2805));
#552=EDGE_LOOP('',(#2806,#2807,#2808,#2809));
#553=EDGE_LOOP('',(#2810,#2811,#2812,#2813));
#554=EDGE_LOOP('',(#2814,#2815,#2816,#2817));
#555=EDGE_LOOP('',(#2818,#2819,#2820,#2821));
#556=EDGE_LOOP('',(#2822));
#557=EDGE_LOOP('',(#2823,#2824,#2825,#2826));
#558=EDGE_LOOP('',(#2827));
#559=EDGE_LOOP('',(#2828,#2829,#2830,#2831));
#560=EDGE_LOOP('',(#2832));
#561=EDGE_LOOP('',(#2833,#2834,#2835,#2836));
#562=EDGE_LOOP('',(#2837));
#563=EDGE_LOOP('',(#2838,#2839,#2840,#2841,#2842,#2843,#2844,#2845));
#564=EDGE_LOOP('',(#2846,#2847,#2848,#2849,#2850,#2851,#2852,#2853));
#565=EDGE_LOOP('',(#2854,#2855,#2856,#2857));
#566=EDGE_LOOP('',(#2858,#2859,#2860,#2861));
#567=EDGE_LOOP('',(#2862,#2863,#2864,#2865));
#568=EDGE_LOOP('',(#2866,#2867,#2868,#2869));
#569=EDGE_LOOP('',(#2870,#2871,#2872,#2873));
#570=EDGE_LOOP('',(#2874,#2875,#2876,#2877));
#571=EDGE_LOOP('',(#2878,#2879,#2880,#2881));
#572=EDGE_LOOP('',(#2882,#2883,#2884,#2885));
#573=EDGE_LOOP('',(#2886,#2887,#2888,#2889));
#574=EDGE_LOOP('',(#2890,#2891,#2892,#2893));
#575=EDGE_LOOP('',(#2894,#2895,#2896,#2897));
#576=EDGE_LOOP('',(#2898,#2899,#2900,#2901,#2902,#2903));
#577=EDGE_LOOP('',(#2904));
#578=EDGE_LOOP('',(#2905,#2906,#2907,#2908,#2909,#2910));
#579=EDGE_LOOP('',(#2911));
#580=EDGE_LOOP('',(#2912,#2913,#2914,#2915));
#581=EDGE_LOOP('',(#2916,#2917,#2918,#2919,#2920,#2921));
#582=EDGE_LOOP('',(#2922));
#583=EDGE_LOOP('',(#2923,#2924,#2925,#2926,#2927,#2928));
#584=EDGE_LOOP('',(#2929));
#585=EDGE_LOOP('',(#2930,#2931,#2932,#2933));
#586=EDGE_LOOP('',(#2934,#2935,#2936,#2937));
#587=EDGE_LOOP('',(#2938,#2939,#2940,#2941,#2942,#2943,#2944,#2945));
#588=EDGE_LOOP('',(#2946,#2947,#2948,#2949,#2950,#2951,#2952,#2953));
#589=EDGE_LOOP('',(#2954,#2955,#2956,#2957));
#590=EDGE_LOOP('',(#2958,#2959,#2960,#2961));
#591=EDGE_LOOP('',(#2962,#2963,#2964,#2965));
#592=EDGE_LOOP('',(#2966,#2967,#2968,#2969));
#593=EDGE_LOOP('',(#2970,#2971,#2972,#2973));
#594=EDGE_LOOP('',(#2974,#2975,#2976,#2977));
#595=EDGE_LOOP('',(#2978,#2979,#2980,#2981));
#596=EDGE_LOOP('',(#2982,#2983,#2984,#2985));
#597=EDGE_LOOP('',(#2986,#2987,#2988,#2989));
#598=EDGE_LOOP('',(#2990,#2991,#2992,#2993));
#599=EDGE_LOOP('',(#2994,#2995,#2996,#2997));
#600=EDGE_LOOP('',(#2998,#2999,#3000,#3001));
#601=LINE('',#4554,#971);
#602=LINE('',#4556,#972);
#603=LINE('',#4558,#973);
#604=LINE('',#4559,#974);
#605=LINE('',#4562,#975);
#606=LINE('',#4564,#976);
#607=LINE('',#4565,#977);
#608=LINE('',#4568,#978);
#609=LINE('',#4570,#979);
#610=LINE('',#4571,#980);
#611=LINE('',#4573,#981);
#612=LINE('',#4574,#982);
#613=LINE('',#4578,#983);
#614=LINE('',#4580,#984);
#615=LINE('',#4582,#985);
#616=LINE('',#4586,#986);
#617=LINE('',#4590,#987);
#618=LINE('',#4592,#988);
#619=LINE('',#4594,#989);
#620=LINE('',#4598,#990);
#621=LINE('',#4603,#991);
#622=LINE('',#4605,#992);
#623=LINE('',#4606,#993);
#624=LINE('',#4608,#994);
#625=LINE('',#4610,#995);
#626=LINE('',#4612,#996);
#627=LINE('',#4614,#997);
#628=LINE('',#4616,#998);
#629=LINE('',#4618,#999);
#630=LINE('',#4620,#1000);
#631=LINE('',#4621,#1001);
#632=LINE('',#4625,#1002);
#633=LINE('',#4627,#1003);
#634=LINE('',#4629,#1004);
#635=LINE('',#4631,#1005);
#636=LINE('',#4633,#1006);
#637=LINE('',#4635,#1007);
#638=LINE('',#4637,#1008);
#639=LINE('',#4639,#1009);
#640=LINE('',#4640,#1010);
#641=LINE('',#4642,#1011);
#642=LINE('',#4643,#1012);
#643=LINE('',#4646,#1013);
#644=LINE('',#4648,#1014);
#645=LINE('',#4652,#1015);
#646=LINE('',#4656,#1016);
#647=LINE('',#4657,#1017);
#648=LINE('',#4661,#1018);
#649=LINE('',#4666,#1019);
#650=LINE('',#4668,#1020);
#651=LINE('',#4669,#1021);
#652=LINE('',#4671,#1022);
#653=LINE('',#4673,#1023);
#654=LINE('',#4675,#1024);
#655=LINE('',#4677,#1025);
#656=LINE('',#4678,#1026);
#657=LINE('',#4680,#1027);
#658=LINE('',#4681,#1028);
#659=LINE('',#4685,#1029);
#660=LINE('',#4687,#1030);
#661=LINE('',#4688,#1031);
#662=LINE('',#4690,#1032);
#663=LINE('',#4692,#1033);
#664=LINE('',#4694,#1034);
#665=LINE('',#4696,#1035);
#666=LINE('',#4697,#1036);
#667=LINE('',#4699,#1037);
#668=LINE('',#4700,#1038);
#669=LINE('',#4704,#1039);
#670=LINE('',#4705,#1040);
#671=LINE('',#4706,#1041);
#672=LINE('',#4711,#1042);
#673=LINE('',#4715,#1043);
#674=LINE('',#4716,#1044);
#675=LINE('',#4719,#1045);
#676=LINE('',#4721,#1046);
#677=LINE('',#4723,#1047);
#678=LINE('',#4724,#1048);
#679=LINE('',#4730,#1049);
#680=LINE('',#4731,#1050);
#681=LINE('',#4735,#1051);
#682=LINE('',#4738,#1052);
#683=LINE('',#4742,#1053);
#684=LINE('',#4744,#1054);
#685=LINE('',#4746,#1055);
#686=LINE('',#4748,#1056);
#687=LINE('',#4750,#1057);
#688=LINE('',#4753,#1058);
#689=LINE('',#4757,#1059);
#690=LINE('',#4759,#1060);
#691=LINE('',#4761,#1061);
#692=LINE('',#4762,#1062);
#693=LINE('',#4764,#1063);
#694=LINE('',#4766,#1064);
#695=LINE('',#4769,#1065);
#696=LINE('',#4771,#1066);
#697=LINE('',#4774,#1067);
#698=LINE('',#4776,#1068);
#699=LINE('',#4779,#1069);
#700=LINE('',#4781,#1070);
#701=LINE('',#4784,#1071);
#702=LINE('',#4785,#1072);
#703=LINE('',#4787,#1073);
#704=LINE('',#4789,#1074);
#705=LINE('',#4795,#1075);
#706=LINE('',#4797,#1076);
#707=LINE('',#4799,#1077);
#708=LINE('',#4800,#1078);
#709=LINE('',#4803,#1079);
#710=LINE('',#4805,#1080);
#711=LINE('',#4807,#1081);
#712=LINE('',#4808,#1082);
#713=LINE('',#4811,#1083);
#714=LINE('',#4813,#1084);
#715=LINE('',#4815,#1085);
#716=LINE('',#4816,#1086);
#717=LINE('',#4820,#1087);
#718=LINE('',#4822,#1088);
#719=LINE('',#4824,#1089);
#720=LINE('',#4825,#1090);
#721=LINE('',#4828,#1091);
#722=LINE('',#4830,#1092);
#723=LINE('',#4832,#1093);
#724=LINE('',#4833,#1094);
#725=LINE('',#4836,#1095);
#726=LINE('',#4838,#1096);
#727=LINE('',#4840,#1097);
#728=LINE('',#4841,#1098);
#729=LINE('',#4845,#1099);
#730=LINE('',#4847,#1100);
#731=LINE('',#4849,#1101);
#732=LINE('',#4850,#1102);
#733=LINE('',#4853,#1103);
#734=LINE('',#4855,#1104);
#735=LINE('',#4856,#1105);
#736=LINE('',#4859,#1106);
#737=LINE('',#4861,#1107);
#738=LINE('',#4862,#1108);
#739=LINE('',#4864,#1109);
#740=LINE('',#4865,#1110);
#741=LINE('',#4869,#1111);
#742=LINE('',#4871,#1112);
#743=LINE('',#4873,#1113);
#744=LINE('',#4874,#1114);
#745=LINE('',#4877,#1115);
#746=LINE('',#4879,#1116);
#747=LINE('',#4880,#1117);
#748=LINE('',#4883,#1118);
#749=LINE('',#4885,#1119);
#750=LINE('',#4886,#1120);
#751=LINE('',#4888,#1121);
#752=LINE('',#4889,#1122);
#753=LINE('',#4893,#1123);
#754=LINE('',#4895,#1124);
#755=LINE('',#4897,#1125);
#756=LINE('',#4898,#1126);
#757=LINE('',#4901,#1127);
#758=LINE('',#4903,#1128);
#759=LINE('',#4905,#1129);
#760=LINE('',#4906,#1130);
#761=LINE('',#4909,#1131);
#762=LINE('',#4911,#1132);
#763=LINE('',#4913,#1133);
#764=LINE('',#4914,#1134);
#765=LINE('',#4918,#1135);
#766=LINE('',#4920,#1136);
#767=LINE('',#4922,#1137);
#768=LINE('',#4923,#1138);
#769=LINE('',#4926,#1139);
#770=LINE('',#4928,#1140);
#771=LINE('',#4930,#1141);
#772=LINE('',#4931,#1142);
#773=LINE('',#4934,#1143);
#774=LINE('',#4936,#1144);
#775=LINE('',#4938,#1145);
#776=LINE('',#4939,#1146);
#777=LINE('',#4943,#1147);
#778=LINE('',#4945,#1148);
#779=LINE('',#4947,#1149);
#780=LINE('',#4948,#1150);
#781=LINE('',#4956,#1151);
#782=LINE('',#4960,#1152);
#783=LINE('',#4962,#1153);
#784=LINE('',#4963,#1154);
#785=LINE('',#4976,#1155);
#786=LINE('',#4980,#1156);
#787=LINE('',#4985,#1157);
#788=LINE('',#4990,#1158);
#789=LINE('',#4993,#1159);
#790=LINE('',#4995,#1160);
#791=LINE('',#4997,#1161);
#792=LINE('',#5000,#1162);
#793=LINE('',#5003,#1163);
#794=LINE('',#5004,#1164);
#795=LINE('',#5006,#1165);
#796=LINE('',#5008,#1166);
#797=LINE('',#5011,#1167);
#798=LINE('',#5012,#1168);
#799=LINE('',#5014,#1169);
#800=LINE('',#5016,#1170);
#801=LINE('',#5019,#1171);
#802=LINE('',#5020,#1172);
#803=LINE('',#5022,#1173);
#804=LINE('',#5024,#1174);
#805=LINE('',#5027,#1175);
#806=LINE('',#5028,#1176);
#807=LINE('',#5030,#1177);
#808=LINE('',#5032,#1178);
#809=LINE('',#5039,#1179);
#810=LINE('',#5046,#1180);
#811=LINE('',#5060,#1181);
#812=LINE('',#5070,#1182);
#813=LINE('',#5076,#1183);
#814=LINE('',#5078,#1184);
#815=LINE('',#5082,#1185);
#816=LINE('',#5086,#1186);
#817=LINE('',#5088,#1187);
#818=LINE('',#5090,#1188);
#819=LINE('',#5094,#1189);
#820=LINE('',#5097,#1190);
#821=LINE('',#5101,#1191);
#822=LINE('',#5105,#1192);
#823=LINE('',#5109,#1193);
#824=LINE('',#5111,#1194);
#825=LINE('',#5113,#1195);
#826=LINE('',#5117,#1196);
#827=LINE('',#5121,#1197);
#828=LINE('',#5122,#1198);
#829=LINE('',#5126,#1199);
#830=LINE('',#5128,#1200);
#831=LINE('',#5129,#1201);
#832=LINE('',#5131,#1202);
#833=LINE('',#5133,#1203);
#834=LINE('',#5135,#1204);
#835=LINE('',#5136,#1205);
#836=LINE('',#5141,#1206);
#837=LINE('',#5145,#1207);
#838=LINE('',#5147,#1208);
#839=LINE('',#5149,#1209);
#840=LINE('',#5151,#1210);
#841=LINE('',#5153,#1211);
#842=LINE('',#5154,#1212);
#843=LINE('',#5156,#1213);
#844=LINE('',#5158,#1214);
#845=LINE('',#5159,#1215);
#846=LINE('',#5161,#1216);
#847=LINE('',#5163,#1217);
#848=LINE('',#5165,#1218);
#849=LINE('',#5166,#1219);
#850=LINE('',#5169,#1220);
#851=LINE('',#5173,#1221);
#852=LINE('',#5175,#1222);
#853=LINE('',#5177,#1223);
#854=LINE('',#5178,#1224);
#855=LINE('',#5180,#1225);
#856=LINE('',#5181,#1226);
#857=LINE('',#5184,#1227);
#858=LINE('',#5188,#1228);
#859=LINE('',#5189,#1229);
#860=LINE('',#5192,#1230);
#861=LINE('',#5196,#1231);
#862=LINE('',#5198,#1232);
#863=LINE('',#5200,#1233);
#864=LINE('',#5201,#1234);
#865=LINE('',#5202,#1235);
#866=LINE('',#5205,#1236);
#867=LINE('',#5209,#1237);
#868=LINE('',#5210,#1238);
#869=LINE('',#5216,#1239);
#870=LINE('',#5221,#1240);
#871=LINE('',#5226,#1241);
#872=LINE('',#5229,#1242);
#873=LINE('',#5230,#1243);
#874=LINE('',#5232,#1244);
#875=LINE('',#5233,#1245);
#876=LINE('',#5235,#1246);
#877=LINE('',#5237,#1247);
#878=LINE('',#5239,#1248);
#879=LINE('',#5241,#1249);
#880=LINE('',#5242,#1250);
#881=LINE('',#5248,#1251);
#882=LINE('',#5249,#1252);
#883=LINE('',#5252,#1253);
#884=LINE('',#5253,#1254);
#885=LINE('',#5255,#1255);
#886=LINE('',#5259,#1256);
#887=LINE('',#5260,#1257);
#888=LINE('',#5263,#1258);
#889=LINE('',#5264,#1259);
#890=LINE('',#5266,#1260);
#891=LINE('',#5269,#1261);
#892=LINE('',#5271,#1262);
#893=LINE('',#5274,#1263);
#894=LINE('',#5276,#1264);
#895=LINE('',#5282,#1265);
#896=LINE('',#5284,#1266);
#897=LINE('',#5286,#1267);
#898=LINE('',#5287,#1268);
#899=LINE('',#5290,#1269);
#900=LINE('',#5292,#1270);
#901=LINE('',#5294,#1271);
#902=LINE('',#5295,#1272);
#903=LINE('',#5298,#1273);
#904=LINE('',#5301,#1274);
#905=LINE('',#5308,#1275);
#906=LINE('',#5309,#1276);
#907=LINE('',#5315,#1277);
#908=LINE('',#5319,#1278);
#909=LINE('',#5320,#1279);
#910=LINE('',#5326,#1280);
#911=LINE('',#5330,#1281);
#912=LINE('',#5331,#1282);
#913=LINE('',#5335,#1283);
#914=LINE('',#5336,#1284);
#915=LINE('',#5337,#1285);
#916=LINE('',#5339,#1286);
#917=LINE('',#5340,#1287);
#918=LINE('',#5341,#1288);
#919=LINE('',#5344,#1289);
#920=LINE('',#5346,#1290);
#921=LINE('',#5351,#1291);
#922=LINE('',#5353,#1292);
#923=LINE('',#5354,#1293);
#924=LINE('',#5357,#1294);
#925=LINE('',#5358,#1295);
#926=LINE('',#5361,#1296);
#927=LINE('',#5362,#1297);
#928=LINE('',#5364,#1298);
#929=LINE('',#5370,#1299);
#930=LINE('',#5372,#1300);
#931=LINE('',#5374,#1301);
#932=LINE('',#5375,#1302);
#933=LINE('',#5379,#1303);
#934=LINE('',#5384,#1304);
#935=LINE('',#5385,#1305);
#936=LINE('',#5393,#1306);
#937=LINE('',#5395,#1307);
#938=LINE('',#5397,#1308);
#939=LINE('',#5400,#1309);
#940=LINE('',#5405,#1310);
#941=LINE('',#5407,#1311);
#942=LINE('',#5408,#1312);
#943=LINE('',#5413,#1313);
#944=LINE('',#5415,#1314);
#945=LINE('',#5417,#1315);
#946=LINE('',#5427,#1316);
#947=LINE('',#5429,#1317);
#948=LINE('',#5430,#1318);
#949=LINE('',#5434,#1319);
#950=LINE('',#5435,#1320);
#951=LINE('',#5438,#1321);
#952=LINE('',#5440,#1322);
#953=LINE('',#5442,#1323);
#954=LINE('',#5443,#1324);
#955=LINE('',#5445,#1325);
#956=LINE('',#5446,#1326);
#957=LINE('',#5447,#1327);
#958=LINE('',#5449,#1328);
#959=LINE('',#5450,#1329);
#960=LINE('',#5451,#1330);
#961=LINE('',#5455,#1331);
#962=LINE('',#5457,#1332);
#963=LINE('',#5458,#1333);
#964=LINE('',#5461,#1334);
#965=LINE('',#5462,#1335);
#966=LINE('',#5465,#1336);
#967=LINE('',#5466,#1337);
#968=LINE('',#5468,#1338);
#969=LINE('',#5475,#1339);
#970=LINE('',#5477,#1340);
#971=VECTOR('',#3651,1000.);
#972=VECTOR('',#3652,1000.);
#973=VECTOR('',#3653,1000.);
#974=VECTOR('',#3654,1000.);
#975=VECTOR('',#3657,1000.);
#976=VECTOR('',#3658,1000.);
#977=VECTOR('',#3659,1000.);
#978=VECTOR('',#3662,1000.);
#979=VECTOR('',#3663,1000.);
#980=VECTOR('',#3664,1000.);
#981=VECTOR('',#3667,1000.);
#982=VECTOR('',#3668,1000.);
#983=VECTOR('',#3671,1000.);
#984=VECTOR('',#3672,1000.);
#985=VECTOR('',#3673,1000.);
#986=VECTOR('',#3676,1000.);
#987=VECTOR('',#3679,1000.);
#988=VECTOR('',#3680,1000.);
#989=VECTOR('',#3681,1000.);
#990=VECTOR('',#3684,1000.);
#991=VECTOR('',#3689,1000.);
#992=VECTOR('',#3690,1000.);
#993=VECTOR('',#3691,1000.);
#994=VECTOR('',#3692,1000.);
#995=VECTOR('',#3693,1000.);
#996=VECTOR('',#3694,1000.);
#997=VECTOR('',#3695,1000.);
#998=VECTOR('',#3696,1000.);
#999=VECTOR('',#3697,1000.);
#1000=VECTOR('',#3698,1000.);
#1001=VECTOR('',#3699,1000.);
#1002=VECTOR('',#3702,1000.);
#1003=VECTOR('',#3703,1000.);
#1004=VECTOR('',#3704,1000.);
#1005=VECTOR('',#3705,1000.);
#1006=VECTOR('',#3706,1000.);
#1007=VECTOR('',#3707,1000.);
#1008=VECTOR('',#3708,1000.);
#1009=VECTOR('',#3709,1000.);
#1010=VECTOR('',#3710,1000.);
#1011=VECTOR('',#3711,1000.);
#1012=VECTOR('',#3712,1000.);
#1013=VECTOR('',#3715,1000.);
#1014=VECTOR('',#3716,1000.);
#1015=VECTOR('',#3719,1000.);
#1016=VECTOR('',#3722,1000.);
#1017=VECTOR('',#3723,1000.);
#1018=VECTOR('',#3726,1000.);
#1019=VECTOR('',#3731,1000.);
#1020=VECTOR('',#3732,1000.);
#1021=VECTOR('',#3733,1000.);
#1022=VECTOR('',#3734,1000.);
#1023=VECTOR('',#3735,1000.);
#1024=VECTOR('',#3736,1000.);
#1025=VECTOR('',#3737,1000.);
#1026=VECTOR('',#3738,1000.);
#1027=VECTOR('',#3739,1000.);
#1028=VECTOR('',#3740,1000.);
#1029=VECTOR('',#3743,1000.);
#1030=VECTOR('',#3744,1000.);
#1031=VECTOR('',#3745,1000.);
#1032=VECTOR('',#3746,1000.);
#1033=VECTOR('',#3747,1000.);
#1034=VECTOR('',#3748,1000.);
#1035=VECTOR('',#3749,1000.);
#1036=VECTOR('',#3750,1000.);
#1037=VECTOR('',#3751,1000.);
#1038=VECTOR('',#3752,1000.);
#1039=VECTOR('',#3755,1000.);
#1040=VECTOR('',#3756,1000.);
#1041=VECTOR('',#3757,1000.);
#1042=VECTOR('',#3764,1000.);
#1043=VECTOR('',#3769,1000.);
#1044=VECTOR('',#3770,1000.);
#1045=VECTOR('',#3771,1000.);
#1046=VECTOR('',#3772,1000.);
#1047=VECTOR('',#3773,1000.);
#1048=VECTOR('',#3774,1000.);
#1049=VECTOR('',#3785,1000.);
#1050=VECTOR('',#3786,1000.);
#1051=VECTOR('',#3789,1000.);
#1052=VECTOR('',#3794,1000.);
#1053=VECTOR('',#3797,1000.);
#1054=VECTOR('',#3800,1000.);
#1055=VECTOR('',#3803,1000.);
#1056=VECTOR('',#3806,1000.);
#1057=VECTOR('',#3809,1000.);
#1058=VECTOR('',#3814,1000.);
#1059=VECTOR('',#3817,1000.);
#1060=VECTOR('',#3818,1000.);
#1061=VECTOR('',#3819,1000.);
#1062=VECTOR('',#3820,1000.);
#1063=VECTOR('',#3823,1000.);
#1064=VECTOR('',#3826,1000.);
#1065=VECTOR('',#3831,1000.);
#1066=VECTOR('',#3834,1000.);
#1067=VECTOR('',#3839,1000.);
#1068=VECTOR('',#3842,1000.);
#1069=VECTOR('',#3847,1000.);
#1070=VECTOR('',#3850,1000.);
#1071=VECTOR('',#3855,1000.);
#1072=VECTOR('',#3856,1000.);
#1073=VECTOR('',#3859,1000.);
#1074=VECTOR('',#3862,1000.);
#1075=VECTOR('',#3869,1000.);
#1076=VECTOR('',#3870,1000.);
#1077=VECTOR('',#3871,1000.);
#1078=VECTOR('',#3872,1000.);
#1079=VECTOR('',#3873,1000.);
#1080=VECTOR('',#3874,1000.);
#1081=VECTOR('',#3875,1000.);
#1082=VECTOR('',#3876,1000.);
#1083=VECTOR('',#3877,1000.);
#1084=VECTOR('',#3878,1000.);
#1085=VECTOR('',#3879,1000.);
#1086=VECTOR('',#3880,1000.);
#1087=VECTOR('',#3883,1000.);
#1088=VECTOR('',#3884,1000.);
#1089=VECTOR('',#3885,1000.);
#1090=VECTOR('',#3886,1000.);
#1091=VECTOR('',#3887,1000.);
#1092=VECTOR('',#3888,1000.);
#1093=VECTOR('',#3889,1000.);
#1094=VECTOR('',#3890,1000.);
#1095=VECTOR('',#3891,1000.);
#1096=VECTOR('',#3892,1000.);
#1097=VECTOR('',#3893,1000.);
#1098=VECTOR('',#3894,1000.);
#1099=VECTOR('',#3897,1000.);
#1100=VECTOR('',#3898,1000.);
#1101=VECTOR('',#3899,1000.);
#1102=VECTOR('',#3900,1000.);
#1103=VECTOR('',#3903,1000.);
#1104=VECTOR('',#3904,1000.);
#1105=VECTOR('',#3905,1000.);
#1106=VECTOR('',#3908,1000.);
#1107=VECTOR('',#3909,1000.);
#1108=VECTOR('',#3910,1000.);
#1109=VECTOR('',#3913,1000.);
#1110=VECTOR('',#3914,1000.);
#1111=VECTOR('',#3917,1000.);
#1112=VECTOR('',#3918,1000.);
#1113=VECTOR('',#3919,1000.);
#1114=VECTOR('',#3920,1000.);
#1115=VECTOR('',#3923,1000.);
#1116=VECTOR('',#3924,1000.);
#1117=VECTOR('',#3925,1000.);
#1118=VECTOR('',#3928,1000.);
#1119=VECTOR('',#3929,1000.);
#1120=VECTOR('',#3930,1000.);
#1121=VECTOR('',#3933,1000.);
#1122=VECTOR('',#3934,1000.);
#1123=VECTOR('',#3937,1000.);
#1124=VECTOR('',#3938,1000.);
#1125=VECTOR('',#3939,1000.);
#1126=VECTOR('',#3940,1000.);
#1127=VECTOR('',#3941,1000.);
#1128=VECTOR('',#3942,1000.);
#1129=VECTOR('',#3943,1000.);
#1130=VECTOR('',#3944,1000.);
#1131=VECTOR('',#3945,1000.);
#1132=VECTOR('',#3946,1000.);
#1133=VECTOR('',#3947,1000.);
#1134=VECTOR('',#3948,1000.);
#1135=VECTOR('',#3951,1000.);
#1136=VECTOR('',#3952,1000.);
#1137=VECTOR('',#3953,1000.);
#1138=VECTOR('',#3954,1000.);
#1139=VECTOR('',#3955,1000.);
#1140=VECTOR('',#3956,1000.);
#1141=VECTOR('',#3957,1000.);
#1142=VECTOR('',#3958,1000.);
#1143=VECTOR('',#3959,1000.);
#1144=VECTOR('',#3960,1000.);
#1145=VECTOR('',#3961,1000.);
#1146=VECTOR('',#3962,1000.);
#1147=VECTOR('',#3965,1000.);
#1148=VECTOR('',#3966,1000.);
#1149=VECTOR('',#3967,1000.);
#1150=VECTOR('',#3968,1000.);
#1151=VECTOR('',#3979,1000.);
#1152=VECTOR('',#3984,1000.);
#1153=VECTOR('',#3985,1000.);
#1154=VECTOR('',#3986,1000.);
#1155=VECTOR('',#4005,1000.);
#1156=VECTOR('',#4010,1000.);
#1157=VECTOR('',#4015,1000.);
#1158=VECTOR('',#4020,1000.);
#1159=VECTOR('',#4025,1000.);
#1160=VECTOR('',#4028,1000.);
#1161=VECTOR('',#4031,1000.);
#1162=VECTOR('',#4036,1000.);
#1163=VECTOR('',#4041,1000.);
#1164=VECTOR('',#4042,1000.);
#1165=VECTOR('',#4045,1000.);
#1166=VECTOR('',#4048,1000.);
#1167=VECTOR('',#4053,1000.);
#1168=VECTOR('',#4054,1000.);
#1169=VECTOR('',#4057,1000.);
#1170=VECTOR('',#4060,1000.);
#1171=VECTOR('',#4065,1000.);
#1172=VECTOR('',#4066,1000.);
#1173=VECTOR('',#4069,1000.);
#1174=VECTOR('',#4072,1000.);
#1175=VECTOR('',#4077,1000.);
#1176=VECTOR('',#4078,1000.);
#1177=VECTOR('',#4081,1000.);
#1178=VECTOR('',#4084,1000.);
#1179=VECTOR('',#4093,5.);
#1180=VECTOR('',#4102,35.);
#1181=VECTOR('',#4121,35.);
#1182=VECTOR('',#4136,5.);
#1183=VECTOR('',#4143,1000.);
#1184=VECTOR('',#4144,1000.);
#1185=VECTOR('',#4147,1000.);
#1186=VECTOR('',#4150,1000.);
#1187=VECTOR('',#4151,1000.);
#1188=VECTOR('',#4152,1000.);
#1189=VECTOR('',#4155,1000.);
#1190=VECTOR('',#4158,1000.);
#1191=VECTOR('',#4161,1000.);
#1192=VECTOR('',#4164,1000.);
#1193=VECTOR('',#4167,1000.);
#1194=VECTOR('',#4168,1000.);
#1195=VECTOR('',#4169,1000.);
#1196=VECTOR('',#4172,1000.);
#1197=VECTOR('',#4175,1000.);
#1198=VECTOR('',#4176,1000.);
#1199=VECTOR('',#4179,1000.);
#1200=VECTOR('',#4180,1000.);
#1201=VECTOR('',#4181,1000.);
#1202=VECTOR('',#4182,1000.);
#1203=VECTOR('',#4183,1000.);
#1204=VECTOR('',#4184,1000.);
#1205=VECTOR('',#4185,1000.);
#1206=VECTOR('',#4190,1000.);
#1207=VECTOR('',#4195,1000.);
#1208=VECTOR('',#4196,1000.);
#1209=VECTOR('',#4197,1000.);
#1210=VECTOR('',#4198,1000.);
#1211=VECTOR('',#4199,1000.);
#1212=VECTOR('',#4200,1000.);
#1213=VECTOR('',#4201,1000.);
#1214=VECTOR('',#4202,1000.);
#1215=VECTOR('',#4203,1000.);
#1216=VECTOR('',#4204,1000.);
#1217=VECTOR('',#4205,1000.);
#1218=VECTOR('',#4206,1000.);
#1219=VECTOR('',#4207,1000.);
#1220=VECTOR('',#4210,1000.);
#1221=VECTOR('',#4215,1000.);
#1222=VECTOR('',#4216,1000.);
#1223=VECTOR('',#4217,1000.);
#1224=VECTOR('',#4218,1000.);
#1225=VECTOR('',#4219,1000.);
#1226=VECTOR('',#4220,1000.);
#1227=VECTOR('',#4223,1000.);
#1228=VECTOR('',#4228,1000.);
#1229=VECTOR('',#4229,1000.);
#1230=VECTOR('',#4232,1000.);
#1231=VECTOR('',#4237,1000.);
#1232=VECTOR('',#4238,1000.);
#1233=VECTOR('',#4239,1000.);
#1234=VECTOR('',#4240,1000.);
#1235=VECTOR('',#4241,1000.);
#1236=VECTOR('',#4244,1000.);
#1237=VECTOR('',#4249,1000.);
#1238=VECTOR('',#4250,1000.);
#1239=VECTOR('',#4257,1000.);
#1240=VECTOR('',#4262,1000.);
#1241=VECTOR('',#4269,1000.);
#1242=VECTOR('',#4272,1000.);
#1243=VECTOR('',#4273,1000.);
#1244=VECTOR('',#4274,1000.);
#1245=VECTOR('',#4275,1000.);
#1246=VECTOR('',#4278,1000.);
#1247=VECTOR('',#4281,1000.);
#1248=VECTOR('',#4282,1000.);
#1249=VECTOR('',#4283,1000.);
#1250=VECTOR('',#4284,1000.);
#1251=VECTOR('',#4293,1000.);
#1252=VECTOR('',#4294,1000.);
#1253=VECTOR('',#4297,1000.);
#1254=VECTOR('',#4298,1000.);
#1255=VECTOR('',#4301,1000.);
#1256=VECTOR('',#4306,1000.);
#1257=VECTOR('',#4307,1000.);
#1258=VECTOR('',#4310,1000.);
#1259=VECTOR('',#4311,1000.);
#1260=VECTOR('',#4314,1000.);
#1261=VECTOR('',#4319,1000.);
#1262=VECTOR('',#4322,1000.);
#1263=VECTOR('',#4327,1000.);
#1264=VECTOR('',#4330,1000.);
#1265=VECTOR('',#4337,1000.);
#1266=VECTOR('',#4338,1000.);
#1267=VECTOR('',#4339,1000.);
#1268=VECTOR('',#4340,1000.);
#1269=VECTOR('',#4341,1000.);
#1270=VECTOR('',#4342,1000.);
#1271=VECTOR('',#4343,1000.);
#1272=VECTOR('',#4344,1000.);
#1273=VECTOR('',#4347,1000.);
#1274=VECTOR('',#4350,1000.);
#1275=VECTOR('',#4357,1000.);
#1276=VECTOR('',#4358,1000.);
#1277=VECTOR('',#4363,1000.);
#1278=VECTOR('',#4366,1000.);
#1279=VECTOR('',#4367,1000.);
#1280=VECTOR('',#4372,1000.);
#1281=VECTOR('',#4375,1000.);
#1282=VECTOR('',#4376,1000.);
#1283=VECTOR('',#4381,1000.);
#1284=VECTOR('',#4382,1000.);
#1285=VECTOR('',#4383,1000.);
#1286=VECTOR('',#4386,1000.);
#1287=VECTOR('',#4387,1000.);
#1288=VECTOR('',#4388,1000.);
#1289=VECTOR('',#4393,4.);
#1290=VECTOR('',#4396,4.);
#1291=VECTOR('',#4403,1000.);
#1292=VECTOR('',#4404,1000.);
#1293=VECTOR('',#4405,1000.);
#1294=VECTOR('',#4408,1000.);
#1295=VECTOR('',#4409,1000.);
#1296=VECTOR('',#4412,1000.);
#1297=VECTOR('',#4413,1000.);
#1298=VECTOR('',#4416,1000.);
#1299=VECTOR('',#4423,1000.);
#1300=VECTOR('',#4424,1000.);
#1301=VECTOR('',#4425,1000.);
#1302=VECTOR('',#4426,1000.);
#1303=VECTOR('',#4429,1000.);
#1304=VECTOR('',#4434,1000.);
#1305=VECTOR('',#4435,1000.);
#1306=VECTOR('',#4442,1000.);
#1307=VECTOR('',#4443,1000.);
#1308=VECTOR('',#4444,1000.);
#1309=VECTOR('',#4447,1000.);
#1310=VECTOR('',#4452,1000.);
#1311=VECTOR('',#4453,1000.);
#1312=VECTOR('',#4454,1000.);
#1313=VECTOR('',#4459,1000.);
#1314=VECTOR('',#4460,1000.);
#1315=VECTOR('',#4461,1000.);
#1316=VECTOR('',#4472,1000.);
#1317=VECTOR('',#4473,1000.);
#1318=VECTOR('',#4474,1000.);
#1319=VECTOR('',#4479,1000.);
#1320=VECTOR('',#4480,1000.);
#1321=VECTOR('',#4481,1000.);
#1322=VECTOR('',#4482,1000.);
#1323=VECTOR('',#4483,1000.);
#1324=VECTOR('',#4484,1000.);
#1325=VECTOR('',#4487,1000.);
#1326=VECTOR('',#4488,1000.);
#1327=VECTOR('',#4489,1000.);
#1328=VECTOR('',#4492,1000.);
#1329=VECTOR('',#4493,1000.);
#1330=VECTOR('',#4494,1000.);
#1331=VECTOR('',#4499,1000.);
#1332=VECTOR('',#4500,1000.);
#1333=VECTOR('',#4501,1000.);
#1334=VECTOR('',#4504,1000.);
#1335=VECTOR('',#4505,1000.);
#1336=VECTOR('',#4508,1000.);
#1337=VECTOR('',#4509,1000.);
#1338=VECTOR('',#4512,1000.);
#1339=VECTOR('',#4525,5.);
#1340=VECTOR('',#4528,5.);
#1341=VERTEX_POINT('',#4552);
#1342=VERTEX_POINT('',#4553);
#1343=VERTEX_POINT('',#4555);
#1344=VERTEX_POINT('',#4557);
#1345=VERTEX_POINT('',#4561);
#1346=VERTEX_POINT('',#4563);
#1347=VERTEX_POINT('',#4567);
#1348=VERTEX_POINT('',#4569);
#1349=VERTEX_POINT('',#4576);
#1350=VERTEX_POINT('',#4577);
#1351=VERTEX_POINT('',#4579);
#1352=VERTEX_POINT('',#4581);
#1353=VERTEX_POINT('',#4583);
#1354=VERTEX_POINT('',#4585);
#1355=VERTEX_POINT('',#4587);
#1356=VERTEX_POINT('',#4589);
#1357=VERTEX_POINT('',#4591);
#1358=VERTEX_POINT('',#4593);
#1359=VERTEX_POINT('',#4595);
#1360=VERTEX_POINT('',#4597);
#1361=VERTEX_POINT('',#4601);
#1362=VERTEX_POINT('',#4602);
#1363=VERTEX_POINT('',#4604);
#1364=VERTEX_POINT('',#4607);
#1365=VERTEX_POINT('',#4609);
#1366=VERTEX_POINT('',#4611);
#1367=VERTEX_POINT('',#4613);
#1368=VERTEX_POINT('',#4615);
#1369=VERTEX_POINT('',#4617);
#1370=VERTEX_POINT('',#4619);
#1371=VERTEX_POINT('',#4623);
#1372=VERTEX_POINT('',#4624);
#1373=VERTEX_POINT('',#4626);
#1374=VERTEX_POINT('',#4628);
#1375=VERTEX_POINT('',#4630);
#1376=VERTEX_POINT('',#4632);
#1377=VERTEX_POINT('',#4634);
#1378=VERTEX_POINT('',#4636);
#1379=VERTEX_POINT('',#4638);
#1380=VERTEX_POINT('',#4641);
#1381=VERTEX_POINT('',#4645);
#1382=VERTEX_POINT('',#4647);
#1383=VERTEX_POINT('',#4649);
#1384=VERTEX_POINT('',#4651);
#1385=VERTEX_POINT('',#4653);
#1386=VERTEX_POINT('',#4655);
#1387=VERTEX_POINT('',#4658);
#1388=VERTEX_POINT('',#4660);
#1389=VERTEX_POINT('',#4664);
#1390=VERTEX_POINT('',#4665);
#1391=VERTEX_POINT('',#4667);
#1392=VERTEX_POINT('',#4670);
#1393=VERTEX_POINT('',#4672);
#1394=VERTEX_POINT('',#4674);
#1395=VERTEX_POINT('',#4676);
#1396=VERTEX_POINT('',#4679);
#1397=VERTEX_POINT('',#4683);
#1398=VERTEX_POINT('',#4684);
#1399=VERTEX_POINT('',#4686);
#1400=VERTEX_POINT('',#4689);
#1401=VERTEX_POINT('',#4691);
#1402=VERTEX_POINT('',#4693);
#1403=VERTEX_POINT('',#4695);
#1404=VERTEX_POINT('',#4698);
#1405=VERTEX_POINT('',#4702);
#1406=VERTEX_POINT('',#4703);
#1407=VERTEX_POINT('',#4710);
#1408=VERTEX_POINT('',#4714);
#1409=VERTEX_POINT('',#4717);
#1410=VERTEX_POINT('',#4718);
#1411=VERTEX_POINT('',#4720);
#1412=VERTEX_POINT('',#4722);
#1413=VERTEX_POINT('',#4732);
#1414=VERTEX_POINT('',#4734);
#1415=VERTEX_POINT('',#4739);
#1416=VERTEX_POINT('',#4741);
#1417=VERTEX_POINT('',#4755);
#1418=VERTEX_POINT('',#4756);
#1419=VERTEX_POINT('',#4758);
#1420=VERTEX_POINT('',#4760);
#1421=VERTEX_POINT('',#4793);
#1422=VERTEX_POINT('',#4794);
#1423=VERTEX_POINT('',#4796);
#1424=VERTEX_POINT('',#4798);
#1425=VERTEX_POINT('',#4801);
#1426=VERTEX_POINT('',#4802);
#1427=VERTEX_POINT('',#4804);
#1428=VERTEX_POINT('',#4806);
#1429=VERTEX_POINT('',#4809);
#1430=VERTEX_POINT('',#4810);
#1431=VERTEX_POINT('',#4812);
#1432=VERTEX_POINT('',#4814);
#1433=VERTEX_POINT('',#4818);
#1434=VERTEX_POINT('',#4819);
#1435=VERTEX_POINT('',#4821);
#1436=VERTEX_POINT('',#4823);
#1437=VERTEX_POINT('',#4826);
#1438=VERTEX_POINT('',#4827);
#1439=VERTEX_POINT('',#4829);
#1440=VERTEX_POINT('',#4831);
#1441=VERTEX_POINT('',#4834);
#1442=VERTEX_POINT('',#4835);
#1443=VERTEX_POINT('',#4837);
#1444=VERTEX_POINT('',#4839);
#1445=VERTEX_POINT('',#4843);
#1446=VERTEX_POINT('',#4844);
#1447=VERTEX_POINT('',#4846);
#1448=VERTEX_POINT('',#4848);
#1449=VERTEX_POINT('',#4852);
#1450=VERTEX_POINT('',#4854);
#1451=VERTEX_POINT('',#4858);
#1452=VERTEX_POINT('',#4860);
#1453=VERTEX_POINT('',#4867);
#1454=VERTEX_POINT('',#4868);
#1455=VERTEX_POINT('',#4870);
#1456=VERTEX_POINT('',#4872);
#1457=VERTEX_POINT('',#4876);
#1458=VERTEX_POINT('',#4878);
#1459=VERTEX_POINT('',#4882);
#1460=VERTEX_POINT('',#4884);
#1461=VERTEX_POINT('',#4891);
#1462=VERTEX_POINT('',#4892);
#1463=VERTEX_POINT('',#4894);
#1464=VERTEX_POINT('',#4896);
#1465=VERTEX_POINT('',#4899);
#1466=VERTEX_POINT('',#4900);
#1467=VERTEX_POINT('',#4902);
#1468=VERTEX_POINT('',#4904);
#1469=VERTEX_POINT('',#4907);
#1470=VERTEX_POINT('',#4908);
#1471=VERTEX_POINT('',#4910);
#1472=VERTEX_POINT('',#4912);
#1473=VERTEX_POINT('',#4916);
#1474=VERTEX_POINT('',#4917);
#1475=VERTEX_POINT('',#4919);
#1476=VERTEX_POINT('',#4921);
#1477=VERTEX_POINT('',#4924);
#1478=VERTEX_POINT('',#4925);
#1479=VERTEX_POINT('',#4927);
#1480=VERTEX_POINT('',#4929);
#1481=VERTEX_POINT('',#4932);
#1482=VERTEX_POINT('',#4933);
#1483=VERTEX_POINT('',#4935);
#1484=VERTEX_POINT('',#4937);
#1485=VERTEX_POINT('',#4941);
#1486=VERTEX_POINT('',#4942);
#1487=VERTEX_POINT('',#4944);
#1488=VERTEX_POINT('',#4946);
#1489=VERTEX_POINT('',#4953);
#1490=VERTEX_POINT('',#4955);
#1491=VERTEX_POINT('',#4959);
#1492=VERTEX_POINT('',#4961);
#1493=VERTEX_POINT('',#4971);
#1494=VERTEX_POINT('',#4973);
#1495=VERTEX_POINT('',#4975);
#1496=VERTEX_POINT('',#4978);
#1497=VERTEX_POINT('',#4982);
#1498=VERTEX_POINT('',#4984);
#1499=VERTEX_POINT('',#4987);
#1500=VERTEX_POINT('',#4989);
#1501=VERTEX_POINT('',#5036);
#1502=VERTEX_POINT('',#5038);
#1503=VERTEX_POINT('',#5042);
#1504=VERTEX_POINT('',#5045);
#1505=VERTEX_POINT('',#5049);
#1506=VERTEX_POINT('',#5052);
#1507=VERTEX_POINT('',#5056);
#1508=VERTEX_POINT('',#5059);
#1509=VERTEX_POINT('',#5065);
#1510=VERTEX_POINT('',#5068);
#1511=VERTEX_POINT('',#5074);
#1512=VERTEX_POINT('',#5075);
#1513=VERTEX_POINT('',#5077);
#1514=VERTEX_POINT('',#5079);
#1515=VERTEX_POINT('',#5081);
#1516=VERTEX_POINT('',#5083);
#1517=VERTEX_POINT('',#5085);
#1518=VERTEX_POINT('',#5087);
#1519=VERTEX_POINT('',#5089);
#1520=VERTEX_POINT('',#5091);
#1521=VERTEX_POINT('',#5093);
#1522=VERTEX_POINT('',#5095);
#1523=VERTEX_POINT('',#5099);
#1524=VERTEX_POINT('',#5100);
#1525=VERTEX_POINT('',#5102);
#1526=VERTEX_POINT('',#5104);
#1527=VERTEX_POINT('',#5106);
#1528=VERTEX_POINT('',#5108);
#1529=VERTEX_POINT('',#5110);
#1530=VERTEX_POINT('',#5112);
#1531=VERTEX_POINT('',#5114);
#1532=VERTEX_POINT('',#5116);
#1533=VERTEX_POINT('',#5118);
#1534=VERTEX_POINT('',#5120);
#1535=VERTEX_POINT('',#5124);
#1536=VERTEX_POINT('',#5125);
#1537=VERTEX_POINT('',#5127);
#1538=VERTEX_POINT('',#5130);
#1539=VERTEX_POINT('',#5132);
#1540=VERTEX_POINT('',#5134);
#1541=VERTEX_POINT('',#5138);
#1542=VERTEX_POINT('',#5140);
#1543=VERTEX_POINT('',#5144);
#1544=VERTEX_POINT('',#5146);
#1545=VERTEX_POINT('',#5148);
#1546=VERTEX_POINT('',#5150);
#1547=VERTEX_POINT('',#5152);
#1548=VERTEX_POINT('',#5155);
#1549=VERTEX_POINT('',#5157);
#1550=VERTEX_POINT('',#5160);
#1551=VERTEX_POINT('',#5162);
#1552=VERTEX_POINT('',#5164);
#1553=VERTEX_POINT('',#5168);
#1554=VERTEX_POINT('',#5172);
#1555=VERTEX_POINT('',#5174);
#1556=VERTEX_POINT('',#5176);
#1557=VERTEX_POINT('',#5179);
#1558=VERTEX_POINT('',#5183);
#1559=VERTEX_POINT('',#5187);
#1560=VERTEX_POINT('',#5191);
#1561=VERTEX_POINT('',#5195);
#1562=VERTEX_POINT('',#5197);
#1563=VERTEX_POINT('',#5199);
#1564=VERTEX_POINT('',#5204);
#1565=VERTEX_POINT('',#5208);
#1566=VERTEX_POINT('',#5214);
#1567=VERTEX_POINT('',#5215);
#1568=VERTEX_POINT('',#5218);
#1569=VERTEX_POINT('',#5220);
#1570=VERTEX_POINT('',#5224);
#1571=VERTEX_POINT('',#5228);
#1572=VERTEX_POINT('',#5231);
#1573=VERTEX_POINT('',#5238);
#1574=VERTEX_POINT('',#5240);
#1575=VERTEX_POINT('',#5247);
#1576=VERTEX_POINT('',#5251);
#1577=VERTEX_POINT('',#5258);
#1578=VERTEX_POINT('',#5262);
#1579=VERTEX_POINT('',#5280);
#1580=VERTEX_POINT('',#5281);
#1581=VERTEX_POINT('',#5283);
#1582=VERTEX_POINT('',#5285);
#1583=VERTEX_POINT('',#5288);
#1584=VERTEX_POINT('',#5289);
#1585=VERTEX_POINT('',#5291);
#1586=VERTEX_POINT('',#5293);
#1587=VERTEX_POINT('',#5297);
#1588=VERTEX_POINT('',#5299);
#1589=VERTEX_POINT('',#5302);
#1590=VERTEX_POINT('',#5305);
#1591=VERTEX_POINT('',#5306);
#1592=VERTEX_POINT('',#5310);
#1593=VERTEX_POINT('',#5313);
#1594=VERTEX_POINT('',#5314);
#1595=VERTEX_POINT('',#5316);
#1596=VERTEX_POINT('',#5318);
#1597=VERTEX_POINT('',#5321);
#1598=VERTEX_POINT('',#5324);
#1599=VERTEX_POINT('',#5325);
#1600=VERTEX_POINT('',#5327);
#1601=VERTEX_POINT('',#5329);
#1602=VERTEX_POINT('',#5332);
#1603=VERTEX_POINT('',#5350);
#1604=VERTEX_POINT('',#5352);
#1605=VERTEX_POINT('',#5356);
#1606=VERTEX_POINT('',#5360);
#1607=VERTEX_POINT('',#5368);
#1608=VERTEX_POINT('',#5369);
#1609=VERTEX_POINT('',#5371);
#1610=VERTEX_POINT('',#5373);
#1611=VERTEX_POINT('',#5377);
#1612=VERTEX_POINT('',#5378);
#1613=VERTEX_POINT('',#5381);
#1614=VERTEX_POINT('',#5383);
#1615=VERTEX_POINT('',#5386);
#1616=VERTEX_POINT('',#5389);
#1617=VERTEX_POINT('',#5390);
#1618=VERTEX_POINT('',#5392);
#1619=VERTEX_POINT('',#5394);
#1620=VERTEX_POINT('',#5396);
#1621=VERTEX_POINT('',#5398);
#1622=VERTEX_POINT('',#5401);
#1623=VERTEX_POINT('',#5404);
#1624=VERTEX_POINT('',#5406);
#1625=VERTEX_POINT('',#5410);
#1626=VERTEX_POINT('',#5412);
#1627=VERTEX_POINT('',#5414);
#1628=VERTEX_POINT('',#5416);
#1629=VERTEX_POINT('',#5419);
#1630=VERTEX_POINT('',#5422);
#1631=VERTEX_POINT('',#5424);
#1632=VERTEX_POINT('',#5426);
#1633=VERTEX_POINT('',#5428);
#1634=VERTEX_POINT('',#5431);
#1635=VERTEX_POINT('',#5436);
#1636=VERTEX_POINT('',#5437);
#1637=VERTEX_POINT('',#5439);
#1638=VERTEX_POINT('',#5441);
#1639=VERTEX_POINT('',#5454);
#1640=VERTEX_POINT('',#5456);
#1641=VERTEX_POINT('',#5460);
#1642=VERTEX_POINT('',#5464);
#1643=EDGE_CURVE('',#1341,#1342,#601,.T.);
#1644=EDGE_CURVE('',#1341,#1343,#602,.T.);
#1645=EDGE_CURVE('',#1343,#1344,#603,.T.);
#1646=EDGE_CURVE('',#1344,#1342,#604,.T.);
#1647=EDGE_CURVE('',#1343,#1345,#605,.T.);
#1648=EDGE_CURVE('',#1345,#1346,#606,.T.);
#1649=EDGE_CURVE('',#1346,#1344,#607,.T.);
#1650=EDGE_CURVE('',#1347,#1345,#608,.T.);
#1651=EDGE_CURVE('',#1347,#1348,#609,.T.);
#1652=EDGE_CURVE('',#1346,#1348,#610,.T.);
#1653=EDGE_CURVE('',#1341,#1347,#611,.T.);
#1654=EDGE_CURVE('',#1348,#1342,#612,.T.);
#1655=EDGE_CURVE('',#1349,#1350,#613,.T.);
#1656=EDGE_CURVE('',#1350,#1351,#614,.T.);
#1657=EDGE_CURVE('',#1351,#1352,#615,.T.);
#1658=EDGE_CURVE('',#1353,#1352,#153,.T.);
#1659=EDGE_CURVE('',#1353,#1354,#616,.T.);
#1660=EDGE_CURVE('',#1355,#1354,#154,.T.);
#1661=EDGE_CURVE('',#1356,#1355,#617,.T.);
#1662=EDGE_CURVE('',#1356,#1357,#618,.T.);
#1663=EDGE_CURVE('',#1357,#1358,#619,.T.);
#1664=EDGE_CURVE('',#1358,#1359,#155,.T.);
#1665=EDGE_CURVE('',#1359,#1360,#620,.T.);
#1666=EDGE_CURVE('',#1360,#1349,#156,.T.);
#1667=EDGE_CURVE('',#1361,#1362,#621,.T.);
#1668=EDGE_CURVE('',#1363,#1361,#622,.T.);
#1669=EDGE_CURVE('',#1363,#1356,#623,.T.);
#1670=EDGE_CURVE('',#1364,#1355,#624,.T.);
#1671=EDGE_CURVE('',#1365,#1364,#625,.F.);
#1672=EDGE_CURVE('',#1366,#1365,#626,.T.);
#1673=EDGE_CURVE('',#1366,#1367,#627,.T.);
#1674=EDGE_CURVE('',#1367,#1368,#628,.T.);
#1675=EDGE_CURVE('',#1369,#1368,#629,.F.);
#1676=EDGE_CURVE('',#1369,#1370,#630,.T.);
#1677=EDGE_CURVE('',#1370,#1362,#631,.T.);
#1678=EDGE_CURVE('',#1371,#1372,#632,.T.);
#1679=EDGE_CURVE('',#1373,#1371,#633,.T.);
#1680=EDGE_CURVE('',#1374,#1373,#634,.T.);
#1681=EDGE_CURVE('',#1374,#1375,#635,.F.);
#1682=EDGE_CURVE('',#1375,#1376,#636,.T.);
#1683=EDGE_CURVE('',#1376,#1377,#637,.T.);
#1684=EDGE_CURVE('',#1378,#1377,#638,.T.);
#1685=EDGE_CURVE('',#1378,#1379,#639,.F.);
#1686=EDGE_CURVE('',#1379,#1352,#640,.T.);
#1687=EDGE_CURVE('',#1351,#1380,#641,.T.);
#1688=EDGE_CURVE('',#1372,#1380,#642,.T.);
#1689=EDGE_CURVE('',#1381,#1368,#643,.F.);
#1690=EDGE_CURVE('',#1382,#1381,#644,.F.);
#1691=EDGE_CURVE('',#1383,#1382,#157,.F.);
#1692=EDGE_CURVE('',#1384,#1383,#645,.F.);
#1693=EDGE_CURVE('',#1385,#1384,#158,.F.);
#1694=EDGE_CURVE('',#1386,#1385,#646,.F.);
#1695=EDGE_CURVE('',#1375,#1386,#647,.F.);
#1696=EDGE_CURVE('',#1374,#1387,#159,.F.);
#1697=EDGE_CURVE('',#1387,#1388,#648,.F.);
#1698=EDGE_CURVE('',#1388,#1369,#160,.F.);
#1699=EDGE_CURVE('',#1389,#1390,#649,.T.);
#1700=EDGE_CURVE('',#1391,#1389,#650,.T.);
#1701=EDGE_CURVE('',#1382,#1391,#651,.T.);
#1702=EDGE_CURVE('',#1381,#1392,#652,.T.);
#1703=EDGE_CURVE('',#1392,#1393,#653,.T.);
#1704=EDGE_CURVE('',#1394,#1393,#654,.T.);
#1705=EDGE_CURVE('',#1394,#1395,#655,.F.);
#1706=EDGE_CURVE('',#1395,#1358,#656,.T.);
#1707=EDGE_CURVE('',#1357,#1396,#657,.T.);
#1708=EDGE_CURVE('',#1390,#1396,#658,.T.);
#1709=EDGE_CURVE('',#1397,#1398,#659,.T.);
#1710=EDGE_CURVE('',#1399,#1397,#660,.T.);
#1711=EDGE_CURVE('',#1399,#1350,#661,.T.);
#1712=EDGE_CURVE('',#1400,#1349,#662,.T.);
#1713=EDGE_CURVE('',#1400,#1401,#663,.F.);
#1714=EDGE_CURVE('',#1402,#1401,#664,.T.);
#1715=EDGE_CURVE('',#1402,#1403,#665,.T.);
#1716=EDGE_CURVE('',#1403,#1386,#666,.T.);
#1717=EDGE_CURVE('',#1385,#1404,#667,.T.);
#1718=EDGE_CURVE('',#1398,#1404,#668,.T.);
#1719=EDGE_CURVE('',#1405,#1406,#669,.T.);
#1720=EDGE_CURVE('',#1384,#1405,#670,.T.);
#1721=EDGE_CURVE('',#1383,#1406,#671,.T.);
#1722=EDGE_CURVE('',#1404,#1405,#161,.T.);
#1723=EDGE_CURVE('',#1407,#1360,#672,.T.);
#1724=EDGE_CURVE('',#1407,#1400,#162,.F.);
#1725=EDGE_CURVE('',#1408,#1359,#673,.T.);
#1726=EDGE_CURVE('',#1408,#1407,#674,.F.);
#1727=EDGE_CURVE('',#1409,#1410,#675,.T.);
#1728=EDGE_CURVE('',#1409,#1411,#676,.T.);
#1729=EDGE_CURVE('',#1411,#1412,#677,.T.);
#1730=EDGE_CURVE('',#1410,#1412,#678,.T.);
#1731=EDGE_CURVE('',#1395,#1408,#163,.F.);
#1732=EDGE_CURVE('',#1406,#1391,#164,.T.);
#1733=EDGE_CURVE('',#1398,#1371,#679,.T.);
#1734=EDGE_CURVE('',#1362,#1389,#680,.T.);
#1735=EDGE_CURVE('',#1413,#1370,#165,.T.);
#1736=EDGE_CURVE('',#1414,#1413,#681,.T.);
#1737=EDGE_CURVE('',#1373,#1414,#166,.T.);
#1738=EDGE_CURVE('',#1394,#1365,#682,.F.);
#1739=EDGE_CURVE('',#1364,#1415,#167,.F.);
#1740=EDGE_CURVE('',#1416,#1415,#683,.F.);
#1741=EDGE_CURVE('',#1416,#1379,#168,.F.);
#1742=EDGE_CURVE('',#1378,#1401,#684,.F.);
#1743=EDGE_CURVE('',#1416,#1353,#685,.T.);
#1744=EDGE_CURVE('',#1387,#1414,#686,.T.);
#1745=EDGE_CURVE('',#1388,#1413,#687,.T.);
#1746=EDGE_CURVE('',#1415,#1354,#688,.T.);
#1747=EDGE_CURVE('',#1417,#1418,#689,.T.);
#1748=EDGE_CURVE('',#1419,#1417,#690,.T.);
#1749=EDGE_CURVE('',#1419,#1420,#691,.T.);
#1750=EDGE_CURVE('',#1420,#1418,#692,.T.);
#1751=EDGE_CURVE('',#1377,#1402,#693,.T.);
#1752=EDGE_CURVE('',#1376,#1403,#694,.T.);
#1753=EDGE_CURVE('',#1392,#1367,#695,.T.);
#1754=EDGE_CURVE('',#1393,#1366,#696,.T.);
#1755=EDGE_CURVE('',#1390,#1361,#697,.T.);
#1756=EDGE_CURVE('',#1396,#1363,#698,.T.);
#1757=EDGE_CURVE('',#1372,#1397,#699,.T.);
#1758=EDGE_CURVE('',#1380,#1399,#700,.T.);
#1759=EDGE_CURVE('',#1418,#1409,#701,.T.);
#1760=EDGE_CURVE('',#1417,#1410,#702,.T.);
#1761=EDGE_CURVE('',#1419,#1412,#703,.T.);
#1762=EDGE_CURVE('',#1420,#1411,#704,.T.);
#1763=EDGE_CURVE('',#1421,#1422,#705,.T.);
#1764=EDGE_CURVE('',#1422,#1423,#706,.T.);
#1765=EDGE_CURVE('',#1424,#1423,#707,.T.);
#1766=EDGE_CURVE('',#1421,#1424,#708,.T.);
#1767=EDGE_CURVE('',#1425,#1426,#709,.T.);
#1768=EDGE_CURVE('',#1425,#1427,#710,.T.);
#1769=EDGE_CURVE('',#1427,#1428,#711,.T.);
#1770=EDGE_CURVE('',#1426,#1428,#712,.T.);
#1771=EDGE_CURVE('',#1429,#1430,#713,.T.);
#1772=EDGE_CURVE('',#1430,#1431,#714,.T.);
#1773=EDGE_CURVE('',#1432,#1431,#715,.T.);
#1774=EDGE_CURVE('',#1429,#1432,#716,.T.);
#1775=EDGE_CURVE('',#1433,#1434,#717,.T.);
#1776=EDGE_CURVE('',#1435,#1434,#718,.T.);
#1777=EDGE_CURVE('',#1436,#1435,#719,.T.);
#1778=EDGE_CURVE('',#1436,#1433,#720,.T.);
#1779=EDGE_CURVE('',#1437,#1438,#721,.T.);
#1780=EDGE_CURVE('',#1438,#1439,#722,.T.);
#1781=EDGE_CURVE('',#1440,#1439,#723,.T.);
#1782=EDGE_CURVE('',#1437,#1440,#724,.T.);
#1783=EDGE_CURVE('',#1441,#1442,#725,.T.);
#1784=EDGE_CURVE('',#1441,#1443,#726,.T.);
#1785=EDGE_CURVE('',#1443,#1444,#727,.T.);
#1786=EDGE_CURVE('',#1442,#1444,#728,.T.);
#1787=EDGE_CURVE('',#1445,#1446,#729,.T.);
#1788=EDGE_CURVE('',#1445,#1447,#730,.T.);
#1789=EDGE_CURVE('',#1447,#1448,#731,.T.);
#1790=EDGE_CURVE('',#1448,#1446,#732,.T.);
#1791=EDGE_CURVE('',#1447,#1449,#733,.T.);
#1792=EDGE_CURVE('',#1449,#1450,#734,.T.);
#1793=EDGE_CURVE('',#1450,#1448,#735,.T.);
#1794=EDGE_CURVE('',#1449,#1451,#736,.T.);
#1795=EDGE_CURVE('',#1451,#1452,#737,.T.);
#1796=EDGE_CURVE('',#1452,#1450,#738,.T.);
#1797=EDGE_CURVE('',#1451,#1445,#739,.T.);
#1798=EDGE_CURVE('',#1446,#1452,#740,.T.);
#1799=EDGE_CURVE('',#1453,#1454,#741,.T.);
#1800=EDGE_CURVE('',#1453,#1455,#742,.T.);
#1801=EDGE_CURVE('',#1455,#1456,#743,.T.);
#1802=EDGE_CURVE('',#1456,#1454,#744,.T.);
#1803=EDGE_CURVE('',#1457,#1455,#745,.T.);
#1804=EDGE_CURVE('',#1457,#1458,#746,.T.);
#1805=EDGE_CURVE('',#1456,#1458,#747,.T.);
#1806=EDGE_CURVE('',#1459,#1457,#748,.T.);
#1807=EDGE_CURVE('',#1459,#1460,#749,.T.);
#1808=EDGE_CURVE('',#1458,#1460,#750,.T.);
#1809=EDGE_CURVE('',#1459,#1453,#751,.T.);
#1810=EDGE_CURVE('',#1454,#1460,#752,.T.);
#1811=EDGE_CURVE('',#1461,#1462,#753,.T.);
#1812=EDGE_CURVE('',#1463,#1462,#754,.T.);
#1813=EDGE_CURVE('',#1464,#1463,#755,.T.);
#1814=EDGE_CURVE('',#1464,#1461,#756,.T.);
#1815=EDGE_CURVE('',#1465,#1466,#757,.T.);
#1816=EDGE_CURVE('',#1466,#1467,#758,.T.);
#1817=EDGE_CURVE('',#1467,#1468,#759,.T.);
#1818=EDGE_CURVE('',#1468,#1465,#760,.T.);
#1819=EDGE_CURVE('',#1469,#1470,#761,.T.);
#1820=EDGE_CURVE('',#1469,#1471,#762,.T.);
#1821=EDGE_CURVE('',#1471,#1472,#763,.T.);
#1822=EDGE_CURVE('',#1470,#1472,#764,.T.);
#1823=EDGE_CURVE('',#1473,#1474,#765,.T.);
#1824=EDGE_CURVE('',#1475,#1474,#766,.F.);
#1825=EDGE_CURVE('',#1476,#1475,#767,.T.);
#1826=EDGE_CURVE('',#1476,#1473,#768,.F.);
#1827=EDGE_CURVE('',#1477,#1478,#769,.T.);
#1828=EDGE_CURVE('',#1478,#1479,#770,.T.);
#1829=EDGE_CURVE('',#1479,#1480,#771,.T.);
#1830=EDGE_CURVE('',#1480,#1477,#772,.T.);
#1831=EDGE_CURVE('',#1481,#1482,#773,.T.);
#1832=EDGE_CURVE('',#1482,#1483,#774,.T.);
#1833=EDGE_CURVE('',#1484,#1483,#775,.T.);
#1834=EDGE_CURVE('',#1481,#1484,#776,.T.);
#1835=EDGE_CURVE('',#1485,#1486,#777,.T.);
#1836=EDGE_CURVE('',#1487,#1485,#778,.T.);
#1837=EDGE_CURVE('',#1487,#1488,#779,.T.);
#1838=EDGE_CURVE('',#1488,#1486,#780,.T.);
#1839=EDGE_CURVE('',#1474,#1485,#169,.T.);
#1840=EDGE_CURVE('',#1473,#1487,#170,.T.);
#1841=EDGE_CURVE('',#1489,#1475,#171,.T.);
#1842=EDGE_CURVE('',#1490,#1489,#781,.T.);
#1843=EDGE_CURVE('',#1490,#1476,#172,.T.);
#1844=EDGE_CURVE('',#1491,#1489,#782,.F.);
#1845=EDGE_CURVE('',#1492,#1491,#783,.T.);
#1846=EDGE_CURVE('',#1492,#1490,#784,.F.);
#1847=EDGE_CURVE('',#1434,#1491,#173,.T.);
#1848=EDGE_CURVE('',#1433,#1492,#174,.T.);
#1849=EDGE_CURVE('',#1486,#1435,#175,.T.);
#1850=EDGE_CURVE('',#1488,#1436,#176,.T.);
#1851=EDGE_CURVE('',#1423,#1493,#177,.T.);
#1852=EDGE_CURVE('',#1494,#1422,#178,.T.);
#1853=EDGE_CURVE('',#1495,#1494,#785,.T.);
#1854=EDGE_CURVE('',#1463,#1495,#179,.T.);
#1855=EDGE_CURVE('',#1496,#1462,#180,.T.);
#1856=EDGE_CURVE('',#1496,#1493,#786,.T.);
#1857=EDGE_CURVE('',#1424,#1497,#181,.T.);
#1858=EDGE_CURVE('',#1498,#1497,#787,.T.);
#1859=EDGE_CURVE('',#1498,#1461,#182,.T.);
#1860=EDGE_CURVE('',#1464,#1499,#183,.T.);
#1861=EDGE_CURVE('',#1499,#1500,#788,.T.);
#1862=EDGE_CURVE('',#1500,#1421,#184,.T.);
#1863=EDGE_CURVE('',#1498,#1496,#789,.T.);
#1864=EDGE_CURVE('',#1499,#1495,#790,.T.);
#1865=EDGE_CURVE('',#1500,#1494,#791,.T.);
#1866=EDGE_CURVE('',#1497,#1493,#792,.T.);
#1867=EDGE_CURVE('',#1466,#1479,#793,.T.);
#1868=EDGE_CURVE('',#1467,#1478,#794,.T.);
#1869=EDGE_CURVE('',#1468,#1477,#795,.T.);
#1870=EDGE_CURVE('',#1465,#1480,#796,.T.);
#1871=EDGE_CURVE('',#1469,#1483,#797,.T.);
#1872=EDGE_CURVE('',#1471,#1482,#798,.T.);
#1873=EDGE_CURVE('',#1472,#1481,#799,.T.);
#1874=EDGE_CURVE('',#1470,#1484,#800,.T.);
#1875=EDGE_CURVE('',#1425,#1439,#801,.T.);
#1876=EDGE_CURVE('',#1427,#1438,#802,.T.);
#1877=EDGE_CURVE('',#1428,#1437,#803,.T.);
#1878=EDGE_CURVE('',#1426,#1440,#804,.T.);
#1879=EDGE_CURVE('',#1430,#1443,#805,.T.);
#1880=EDGE_CURVE('',#1431,#1441,#806,.T.);
#1881=EDGE_CURVE('',#1432,#1442,#807,.T.);
#1882=EDGE_CURVE('',#1429,#1444,#808,.T.);
#1883=EDGE_CURVE('',#1501,#1501,#185,.T.);
#1884=EDGE_CURVE('',#1501,#1502,#809,.T.);
#1885=EDGE_CURVE('',#1502,#1502,#186,.T.);
#1886=EDGE_CURVE('',#1503,#1503,#187,.T.);
#1887=EDGE_CURVE('',#1503,#1504,#810,.T.);
#1888=EDGE_CURVE('',#1504,#1504,#188,.T.);
#1889=EDGE_CURVE('',#1505,#1505,#189,.T.);
#1890=EDGE_CURVE('',#1505,#1506,#190,.T.);
#1891=EDGE_CURVE('',#1506,#1506,#191,.T.);
#1892=EDGE_CURVE('',#1507,#1507,#192,.T.);
#1893=EDGE_CURVE('',#1507,#1508,#811,.T.);
#1894=EDGE_CURVE('',#1508,#1508,#193,.T.);
#1895=EDGE_CURVE('',#1509,#1509,#194,.T.);
#1896=EDGE_CURVE('',#1510,#1510,#195,.T.);
#1897=EDGE_CURVE('',#1510,#1509,#812,.T.);
#1898=EDGE_CURVE('',#1511,#1512,#813,.T.);
#1899=EDGE_CURVE('',#1512,#1513,#814,.T.);
#1900=EDGE_CURVE('',#1514,#1513,#196,.T.);
#1901=EDGE_CURVE('',#1515,#1514,#815,.T.);
#1902=EDGE_CURVE('',#1516,#1515,#197,.T.);
#1903=EDGE_CURVE('',#1517,#1516,#816,.T.);
#1904=EDGE_CURVE('',#1517,#1518,#817,.T.);
#1905=EDGE_CURVE('',#1518,#1519,#818,.T.);
#1906=EDGE_CURVE('',#1519,#1520,#198,.T.);
#1907=EDGE_CURVE('',#1520,#1521,#819,.T.);
#1908=EDGE_CURVE('',#1521,#1522,#199,.T.);
#1909=EDGE_CURVE('',#1522,#1511,#820,.F.);
#1910=EDGE_CURVE('',#1523,#1524,#821,.F.);
#1911=EDGE_CURVE('',#1524,#1525,#200,.T.);
#1912=EDGE_CURVE('',#1525,#1526,#822,.F.);
#1913=EDGE_CURVE('',#1526,#1527,#201,.T.);
#1914=EDGE_CURVE('',#1527,#1528,#823,.T.);
#1915=EDGE_CURVE('',#1529,#1528,#824,.T.);
#1916=EDGE_CURVE('',#1530,#1529,#825,.T.);
#1917=EDGE_CURVE('',#1531,#1530,#202,.T.);
#1918=EDGE_CURVE('',#1531,#1532,#826,.T.);
#1919=EDGE_CURVE('',#1533,#1532,#203,.T.);
#1920=EDGE_CURVE('',#1533,#1534,#827,.T.);
#1921=EDGE_CURVE('',#1523,#1534,#828,.T.);
#1922=EDGE_CURVE('',#1535,#1536,#829,.T.);
#1923=EDGE_CURVE('',#1535,#1537,#830,.T.);
#1924=EDGE_CURVE('',#1526,#1537,#831,.T.);
#1925=EDGE_CURVE('',#1525,#1538,#832,.T.);
#1926=EDGE_CURVE('',#1538,#1539,#833,.T.);
#1927=EDGE_CURVE('',#1540,#1539,#834,.T.);
#1928=EDGE_CURVE('',#1536,#1540,#835,.T.);
#1929=EDGE_CURVE('',#1539,#1541,#204,.T.);
#1930=EDGE_CURVE('',#1542,#1541,#836,.T.);
#1931=EDGE_CURVE('',#1540,#1542,#205,.F.);
#1932=EDGE_CURVE('',#1541,#1543,#837,.T.);
#1933=EDGE_CURVE('',#1544,#1543,#838,.T.);
#1934=EDGE_CURVE('',#1544,#1545,#839,.T.);
#1935=EDGE_CURVE('',#1545,#1546,#840,.T.);
#1936=EDGE_CURVE('',#1547,#1546,#841,.T.);
#1937=EDGE_CURVE('',#1519,#1547,#842,.T.);
#1938=EDGE_CURVE('',#1548,#1518,#843,.T.);
#1939=EDGE_CURVE('',#1548,#1549,#844,.T.);
#1940=EDGE_CURVE('',#1549,#1528,#845,.T.);
#1941=EDGE_CURVE('',#1527,#1550,#846,.T.);
#1942=EDGE_CURVE('',#1550,#1551,#847,.T.);
#1943=EDGE_CURVE('',#1552,#1551,#848,.T.);
#1944=EDGE_CURVE('',#1542,#1552,#849,.T.);
#1945=EDGE_CURVE('',#1520,#1553,#850,.T.);
#1946=EDGE_CURVE('',#1553,#1547,#206,.F.);
#1947=EDGE_CURVE('',#1513,#1554,#851,.T.);
#1948=EDGE_CURVE('',#1555,#1512,#852,.T.);
#1949=EDGE_CURVE('',#1555,#1556,#853,.T.);
#1950=EDGE_CURVE('',#1556,#1534,#854,.T.);
#1951=EDGE_CURVE('',#1533,#1557,#855,.T.);
#1952=EDGE_CURVE('',#1557,#1554,#856,.T.);
#1953=EDGE_CURVE('',#1514,#1558,#857,.T.);
#1954=EDGE_CURVE('',#1558,#1554,#207,.T.);
#1955=EDGE_CURVE('',#1515,#1559,#858,.T.);
#1956=EDGE_CURVE('',#1559,#1558,#859,.T.);
#1957=EDGE_CURVE('',#1516,#1560,#860,.T.);
#1958=EDGE_CURVE('',#1560,#1559,#208,.T.);
#1959=EDGE_CURVE('',#1530,#1561,#861,.T.);
#1960=EDGE_CURVE('',#1562,#1529,#862,.T.);
#1961=EDGE_CURVE('',#1563,#1562,#863,.T.);
#1962=EDGE_CURVE('',#1563,#1517,#864,.T.);
#1963=EDGE_CURVE('',#1561,#1560,#865,.T.);
#1964=EDGE_CURVE('',#1531,#1564,#866,.T.);
#1965=EDGE_CURVE('',#1564,#1561,#209,.T.);
#1966=EDGE_CURVE('',#1532,#1565,#867,.T.);
#1967=EDGE_CURVE('',#1564,#1565,#868,.T.);
#1968=EDGE_CURVE('',#1557,#1565,#210,.T.);
#1969=EDGE_CURVE('',#1566,#1567,#869,.T.);
#1970=EDGE_CURVE('',#1543,#1566,#211,.T.);
#1971=EDGE_CURVE('',#1568,#1538,#212,.T.);
#1972=EDGE_CURVE('',#1569,#1568,#870,.T.);
#1973=EDGE_CURVE('',#1567,#1569,#213,.T.);
#1974=EDGE_CURVE('',#1570,#1544,#214,.F.);
#1975=EDGE_CURVE('',#1570,#1566,#871,.T.);
#1976=EDGE_CURVE('',#1571,#1570,#872,.T.);
#1977=EDGE_CURVE('',#1521,#1567,#873,.T.);
#1978=EDGE_CURVE('',#1572,#1553,#874,.T.);
#1979=EDGE_CURVE('',#1572,#1571,#875,.T.);
#1980=EDGE_CURVE('',#1522,#1569,#876,.T.);
#1981=EDGE_CURVE('',#1524,#1568,#877,.T.);
#1982=EDGE_CURVE('',#1573,#1523,#878,.T.);
#1983=EDGE_CURVE('',#1574,#1573,#879,.T.);
#1984=EDGE_CURVE('',#1574,#1511,#880,.T.);
#1985=EDGE_CURVE('',#1537,#1550,#215,.F.);
#1986=EDGE_CURVE('',#1575,#1571,#881,.T.);
#1987=EDGE_CURVE('',#1575,#1545,#882,.T.);
#1988=EDGE_CURVE('',#1576,#1572,#883,.T.);
#1989=EDGE_CURVE('',#1576,#1575,#884,.T.);
#1990=EDGE_CURVE('',#1576,#1546,#885,.T.);
#1991=EDGE_CURVE('',#1577,#1552,#886,.T.);
#1992=EDGE_CURVE('',#1577,#1536,#887,.T.);
#1993=EDGE_CURVE('',#1578,#1577,#888,.T.);
#1994=EDGE_CURVE('',#1578,#1535,#889,.T.);
#1995=EDGE_CURVE('',#1578,#1551,#890,.T.);
#1996=EDGE_CURVE('',#1563,#1548,#891,.T.);
#1997=EDGE_CURVE('',#1562,#1549,#892,.T.);
#1998=EDGE_CURVE('',#1574,#1555,#893,.T.);
#1999=EDGE_CURVE('',#1573,#1556,#894,.T.);
#2000=EDGE_CURVE('',#1579,#1580,#895,.T.);
#2001=EDGE_CURVE('',#1581,#1580,#896,.T.);
#2002=EDGE_CURVE('',#1582,#1581,#897,.T.);
#2003=EDGE_CURVE('',#1582,#1579,#898,.T.);
#2004=EDGE_CURVE('',#1583,#1584,#899,.T.);
#2005=EDGE_CURVE('',#1583,#1585,#900,.T.);
#2006=EDGE_CURVE('',#1585,#1586,#901,.T.);
#2007=EDGE_CURVE('',#1584,#1586,#902,.T.);
#2008=EDGE_CURVE('',#1587,#1579,#903,.T.);
#2009=EDGE_CURVE('',#1587,#1588,#216,.T.);
#2010=EDGE_CURVE('',#1588,#1580,#904,.T.);
#2011=EDGE_CURVE('',#1589,#1589,#217,.T.);
#2012=EDGE_CURVE('',#1590,#1591,#218,.T.);
#2013=EDGE_CURVE('',#1590,#1582,#905,.T.);
#2014=EDGE_CURVE('',#1591,#1581,#906,.T.);
#2015=EDGE_CURVE('',#1592,#1592,#219,.T.);
#2016=EDGE_CURVE('',#1593,#1594,#907,.T.);
#2017=EDGE_CURVE('',#1594,#1595,#220,.T.);
#2018=EDGE_CURVE('',#1596,#1595,#908,.T.);
#2019=EDGE_CURVE('',#1596,#1593,#909,.T.);
#2020=EDGE_CURVE('',#1597,#1597,#221,.T.);
#2021=EDGE_CURVE('',#1598,#1599,#910,.T.);
#2022=EDGE_CURVE('',#1600,#1599,#222,.T.);
#2023=EDGE_CURVE('',#1601,#1600,#911,.T.);
#2024=EDGE_CURVE('',#1598,#1601,#912,.T.);
#2025=EDGE_CURVE('',#1602,#1602,#223,.T.);
#2026=EDGE_CURVE('',#1595,#1587,#913,.T.);
#2027=EDGE_CURVE('',#1590,#1599,#914,.T.);
#2028=EDGE_CURVE('',#1598,#1596,#915,.T.);
#2029=EDGE_CURVE('',#1594,#1588,#916,.T.);
#2030=EDGE_CURVE('',#1601,#1593,#917,.T.);
#2031=EDGE_CURVE('',#1591,#1600,#918,.T.);
#2032=EDGE_CURVE('',#1592,#1602,#919,.T.);
#2033=EDGE_CURVE('',#1597,#1589,#920,.T.);
#2034=EDGE_CURVE('',#1603,#1584,#921,.T.);
#2035=EDGE_CURVE('',#1604,#1603,#922,.T.);
#2036=EDGE_CURVE('',#1604,#1583,#923,.T.);
#2037=EDGE_CURVE('',#1604,#1605,#924,.T.);
#2038=EDGE_CURVE('',#1605,#1585,#925,.T.);
#2039=EDGE_CURVE('',#1605,#1606,#926,.T.);
#2040=EDGE_CURVE('',#1606,#1586,#927,.T.);
#2041=EDGE_CURVE('',#1603,#1606,#928,.T.);
#2042=EDGE_CURVE('',#1607,#1608,#929,.T.);
#2043=EDGE_CURVE('',#1608,#1609,#930,.T.);
#2044=EDGE_CURVE('',#1610,#1609,#931,.T.);
#2045=EDGE_CURVE('',#1607,#1610,#932,.T.);
#2046=EDGE_CURVE('',#1611,#1612,#933,.T.);
#2047=EDGE_CURVE('',#1611,#1610,#224,.T.);
#2048=EDGE_CURVE('',#1609,#1613,#225,.T.);
#2049=EDGE_CURVE('',#1613,#1614,#934,.T.);
#2050=EDGE_CURVE('',#1612,#1614,#935,.T.);
#2051=EDGE_CURVE('',#1615,#1615,#226,.T.);
#2052=EDGE_CURVE('',#1616,#1617,#227,.T.);
#2053=EDGE_CURVE('',#1616,#1618,#936,.T.);
#2054=EDGE_CURVE('',#1618,#1619,#937,.T.);
#2055=EDGE_CURVE('',#1620,#1619,#938,.T.);
#2056=EDGE_CURVE('',#1621,#1620,#228,.T.);
#2057=EDGE_CURVE('',#1617,#1621,#939,.T.);
#2058=EDGE_CURVE('',#1622,#1622,#229,.T.);
#2059=EDGE_CURVE('',#1621,#1623,#940,.T.);
#2060=EDGE_CURVE('',#1624,#1623,#941,.T.);
#2061=EDGE_CURVE('',#1617,#1624,#942,.T.);
#2062=EDGE_CURVE('',#1607,#1625,#230,.T.);
#2063=EDGE_CURVE('',#1626,#1625,#943,.T.);
#2064=EDGE_CURVE('',#1627,#1626,#944,.T.);
#2065=EDGE_CURVE('',#1628,#1627,#945,.T.);
#2066=EDGE_CURVE('',#1628,#1608,#231,.T.);
#2067=EDGE_CURVE('',#1629,#1629,#232,.T.);
#2068=EDGE_CURVE('',#1624,#1630,#233,.T.);
#2069=EDGE_CURVE('',#1631,#1623,#234,.T.);
#2070=EDGE_CURVE('',#1631,#1632,#946,.T.);
#2071=EDGE_CURVE('',#1632,#1633,#947,.T.);
#2072=EDGE_CURVE('',#1633,#1630,#948,.T.);
#2073=EDGE_CURVE('',#1634,#1634,#235,.T.);
#2074=EDGE_CURVE('',#1614,#1619,#949,.T.);
#2075=EDGE_CURVE('',#1612,#1618,#950,.T.);
#2076=EDGE_CURVE('',#1635,#1636,#951,.T.);
#2077=EDGE_CURVE('',#1635,#1637,#952,.T.);
#2078=EDGE_CURVE('',#1637,#1638,#953,.T.);
#2079=EDGE_CURVE('',#1636,#1638,#954,.T.);
#2080=EDGE_CURVE('',#1620,#1631,#955,.T.);
#2081=EDGE_CURVE('',#1628,#1613,#956,.T.);
#2082=EDGE_CURVE('',#1632,#1627,#957,.T.);
#2083=EDGE_CURVE('',#1616,#1630,#958,.T.);
#2084=EDGE_CURVE('',#1626,#1633,#959,.T.);
#2085=EDGE_CURVE('',#1625,#1611,#960,.T.);
#2086=EDGE_CURVE('',#1639,#1636,#961,.T.);
#2087=EDGE_CURVE('',#1640,#1639,#962,.T.);
#2088=EDGE_CURVE('',#1640,#1635,#963,.T.);
#2089=EDGE_CURVE('',#1641,#1638,#964,.T.);
#2090=EDGE_CURVE('',#1639,#1641,#965,.T.);
#2091=EDGE_CURVE('',#1642,#1637,#966,.T.);
#2092=EDGE_CURVE('',#1642,#1641,#967,.T.);
#2093=EDGE_CURVE('',#1640,#1642,#968,.T.);
#2094=EDGE_CURVE('',#1622,#1634,#969,.T.);
#2095=EDGE_CURVE('',#1629,#1615,#970,.T.);
#2096=ORIENTED_EDGE('',*,*,#1643,.F.);
#2097=ORIENTED_EDGE('',*,*,#1644,.T.);
#2098=ORIENTED_EDGE('',*,*,#1645,.T.);
#2099=ORIENTED_EDGE('',*,*,#1646,.T.);
#2100=ORIENTED_EDGE('',*,*,#1645,.F.);
#2101=ORIENTED_EDGE('',*,*,#1647,.T.);
#2102=ORIENTED_EDGE('',*,*,#1648,.T.);
#2103=ORIENTED_EDGE('',*,*,#1649,.T.);
#2104=ORIENTED_EDGE('',*,*,#1650,.F.);
#2105=ORIENTED_EDGE('',*,*,#1651,.T.);
#2106=ORIENTED_EDGE('',*,*,#1652,.F.);
#2107=ORIENTED_EDGE('',*,*,#1648,.F.);
#2108=ORIENTED_EDGE('',*,*,#1653,.F.);
#2109=ORIENTED_EDGE('',*,*,#1643,.T.);
#2110=ORIENTED_EDGE('',*,*,#1654,.F.);
#2111=ORIENTED_EDGE('',*,*,#1651,.F.);
#2112=ORIENTED_EDGE('',*,*,#1655,.T.);
#2113=ORIENTED_EDGE('',*,*,#1656,.T.);
#2114=ORIENTED_EDGE('',*,*,#1657,.T.);
#2115=ORIENTED_EDGE('',*,*,#1658,.F.);
#2116=ORIENTED_EDGE('',*,*,#1659,.T.);
#2117=ORIENTED_EDGE('',*,*,#1660,.F.);
#2118=ORIENTED_EDGE('',*,*,#1661,.F.);
#2119=ORIENTED_EDGE('',*,*,#1662,.T.);
#2120=ORIENTED_EDGE('',*,*,#1663,.T.);
#2121=ORIENTED_EDGE('',*,*,#1664,.T.);
#2122=ORIENTED_EDGE('',*,*,#1665,.T.);
#2123=ORIENTED_EDGE('',*,*,#1666,.T.);
#2124=ORIENTED_EDGE('',*,*,#1667,.F.);
#2125=ORIENTED_EDGE('',*,*,#1668,.F.);
#2126=ORIENTED_EDGE('',*,*,#1669,.T.);
#2127=ORIENTED_EDGE('',*,*,#1661,.T.);
#2128=ORIENTED_EDGE('',*,*,#1670,.F.);
#2129=ORIENTED_EDGE('',*,*,#1671,.F.);
#2130=ORIENTED_EDGE('',*,*,#1672,.F.);
#2131=ORIENTED_EDGE('',*,*,#1673,.T.);
#2132=ORIENTED_EDGE('',*,*,#1674,.T.);
#2133=ORIENTED_EDGE('',*,*,#1675,.F.);
#2134=ORIENTED_EDGE('',*,*,#1676,.T.);
#2135=ORIENTED_EDGE('',*,*,#1677,.T.);
#2136=ORIENTED_EDGE('',*,*,#1678,.F.);
#2137=ORIENTED_EDGE('',*,*,#1679,.F.);
#2138=ORIENTED_EDGE('',*,*,#1680,.F.);
#2139=ORIENTED_EDGE('',*,*,#1681,.T.);
#2140=ORIENTED_EDGE('',*,*,#1682,.T.);
#2141=ORIENTED_EDGE('',*,*,#1683,.T.);
#2142=ORIENTED_EDGE('',*,*,#1684,.F.);
#2143=ORIENTED_EDGE('',*,*,#1685,.T.);
#2144=ORIENTED_EDGE('',*,*,#1686,.T.);
#2145=ORIENTED_EDGE('',*,*,#1657,.F.);
#2146=ORIENTED_EDGE('',*,*,#1687,.T.);
#2147=ORIENTED_EDGE('',*,*,#1688,.F.);
#2148=ORIENTED_EDGE('',*,*,#1689,.F.);
#2149=ORIENTED_EDGE('',*,*,#1690,.F.);
#2150=ORIENTED_EDGE('',*,*,#1691,.F.);
#2151=ORIENTED_EDGE('',*,*,#1692,.F.);
#2152=ORIENTED_EDGE('',*,*,#1693,.F.);
#2153=ORIENTED_EDGE('',*,*,#1694,.F.);
#2154=ORIENTED_EDGE('',*,*,#1695,.F.);
#2155=ORIENTED_EDGE('',*,*,#1681,.F.);
#2156=ORIENTED_EDGE('',*,*,#1696,.T.);
#2157=ORIENTED_EDGE('',*,*,#1697,.T.);
#2158=ORIENTED_EDGE('',*,*,#1698,.T.);
#2159=ORIENTED_EDGE('',*,*,#1675,.T.);
#2160=ORIENTED_EDGE('',*,*,#1699,.F.);
#2161=ORIENTED_EDGE('',*,*,#1700,.F.);
#2162=ORIENTED_EDGE('',*,*,#1701,.F.);
#2163=ORIENTED_EDGE('',*,*,#1690,.T.);
#2164=ORIENTED_EDGE('',*,*,#1702,.T.);
#2165=ORIENTED_EDGE('',*,*,#1703,.T.);
#2166=ORIENTED_EDGE('',*,*,#1704,.F.);
#2167=ORIENTED_EDGE('',*,*,#1705,.T.);
#2168=ORIENTED_EDGE('',*,*,#1706,.T.);
#2169=ORIENTED_EDGE('',*,*,#1663,.F.);
#2170=ORIENTED_EDGE('',*,*,#1707,.T.);
#2171=ORIENTED_EDGE('',*,*,#1708,.F.);
#2172=ORIENTED_EDGE('',*,*,#1709,.F.);
#2173=ORIENTED_EDGE('',*,*,#1710,.F.);
#2174=ORIENTED_EDGE('',*,*,#1711,.T.);
#2175=ORIENTED_EDGE('',*,*,#1655,.F.);
#2176=ORIENTED_EDGE('',*,*,#1712,.F.);
#2177=ORIENTED_EDGE('',*,*,#1713,.T.);
#2178=ORIENTED_EDGE('',*,*,#1714,.F.);
#2179=ORIENTED_EDGE('',*,*,#1715,.T.);
#2180=ORIENTED_EDGE('',*,*,#1716,.T.);
#2181=ORIENTED_EDGE('',*,*,#1694,.T.);
#2182=ORIENTED_EDGE('',*,*,#1717,.T.);
#2183=ORIENTED_EDGE('',*,*,#1718,.F.);
#2184=ORIENTED_EDGE('',*,*,#1719,.F.);
#2185=ORIENTED_EDGE('',*,*,#1720,.F.);
#2186=ORIENTED_EDGE('',*,*,#1692,.T.);
#2187=ORIENTED_EDGE('',*,*,#1721,.T.);
#2188=ORIENTED_EDGE('',*,*,#1720,.T.);
#2189=ORIENTED_EDGE('',*,*,#1722,.F.);
#2190=ORIENTED_EDGE('',*,*,#1717,.F.);
#2191=ORIENTED_EDGE('',*,*,#1693,.T.);
#2192=ORIENTED_EDGE('',*,*,#1712,.T.);
#2193=ORIENTED_EDGE('',*,*,#1666,.F.);
#2194=ORIENTED_EDGE('',*,*,#1723,.F.);
#2195=ORIENTED_EDGE('',*,*,#1724,.T.);
#2196=ORIENTED_EDGE('',*,*,#1723,.T.);
#2197=ORIENTED_EDGE('',*,*,#1665,.F.);
#2198=ORIENTED_EDGE('',*,*,#1725,.F.);
#2199=ORIENTED_EDGE('',*,*,#1726,.T.);
#2200=ORIENTED_EDGE('',*,*,#1652,.T.);
#2201=ORIENTED_EDGE('',*,*,#1654,.T.);
#2202=ORIENTED_EDGE('',*,*,#1646,.F.);
#2203=ORIENTED_EDGE('',*,*,#1649,.F.);
#2204=ORIENTED_EDGE('',*,*,#1727,.F.);
#2205=ORIENTED_EDGE('',*,*,#1728,.T.);
#2206=ORIENTED_EDGE('',*,*,#1729,.T.);
#2207=ORIENTED_EDGE('',*,*,#1730,.F.);
#2208=ORIENTED_EDGE('',*,*,#1725,.T.);
#2209=ORIENTED_EDGE('',*,*,#1664,.F.);
#2210=ORIENTED_EDGE('',*,*,#1706,.F.);
#2211=ORIENTED_EDGE('',*,*,#1731,.T.);
#2212=ORIENTED_EDGE('',*,*,#1701,.T.);
#2213=ORIENTED_EDGE('',*,*,#1732,.F.);
#2214=ORIENTED_EDGE('',*,*,#1721,.F.);
#2215=ORIENTED_EDGE('',*,*,#1691,.T.);
#2216=ORIENTED_EDGE('',*,*,#1733,.F.);
#2217=ORIENTED_EDGE('',*,*,#1718,.T.);
#2218=ORIENTED_EDGE('',*,*,#1722,.T.);
#2219=ORIENTED_EDGE('',*,*,#1719,.T.);
#2220=ORIENTED_EDGE('',*,*,#1732,.T.);
#2221=ORIENTED_EDGE('',*,*,#1700,.T.);
#2222=ORIENTED_EDGE('',*,*,#1734,.F.);
#2223=ORIENTED_EDGE('',*,*,#1677,.F.);
#2224=ORIENTED_EDGE('',*,*,#1735,.F.);
#2225=ORIENTED_EDGE('',*,*,#1736,.F.);
#2226=ORIENTED_EDGE('',*,*,#1737,.F.);
#2227=ORIENTED_EDGE('',*,*,#1679,.T.);
#2228=ORIENTED_EDGE('',*,*,#1705,.F.);
#2229=ORIENTED_EDGE('',*,*,#1738,.T.);
#2230=ORIENTED_EDGE('',*,*,#1671,.T.);
#2231=ORIENTED_EDGE('',*,*,#1739,.T.);
#2232=ORIENTED_EDGE('',*,*,#1740,.F.);
#2233=ORIENTED_EDGE('',*,*,#1741,.T.);
#2234=ORIENTED_EDGE('',*,*,#1685,.F.);
#2235=ORIENTED_EDGE('',*,*,#1742,.T.);
#2236=ORIENTED_EDGE('',*,*,#1713,.F.);
#2237=ORIENTED_EDGE('',*,*,#1724,.F.);
#2238=ORIENTED_EDGE('',*,*,#1726,.F.);
#2239=ORIENTED_EDGE('',*,*,#1731,.F.);
#2240=ORIENTED_EDGE('',*,*,#1658,.T.);
#2241=ORIENTED_EDGE('',*,*,#1686,.F.);
#2242=ORIENTED_EDGE('',*,*,#1741,.F.);
#2243=ORIENTED_EDGE('',*,*,#1743,.T.);
#2244=ORIENTED_EDGE('',*,*,#1680,.T.);
#2245=ORIENTED_EDGE('',*,*,#1737,.T.);
#2246=ORIENTED_EDGE('',*,*,#1744,.F.);
#2247=ORIENTED_EDGE('',*,*,#1696,.F.);
#2248=ORIENTED_EDGE('',*,*,#1744,.T.);
#2249=ORIENTED_EDGE('',*,*,#1736,.T.);
#2250=ORIENTED_EDGE('',*,*,#1745,.F.);
#2251=ORIENTED_EDGE('',*,*,#1697,.F.);
#2252=ORIENTED_EDGE('',*,*,#1745,.T.);
#2253=ORIENTED_EDGE('',*,*,#1735,.T.);
#2254=ORIENTED_EDGE('',*,*,#1676,.F.);
#2255=ORIENTED_EDGE('',*,*,#1698,.F.);
#2256=ORIENTED_EDGE('',*,*,#1670,.T.);
#2257=ORIENTED_EDGE('',*,*,#1660,.T.);
#2258=ORIENTED_EDGE('',*,*,#1746,.F.);
#2259=ORIENTED_EDGE('',*,*,#1739,.F.);
#2260=ORIENTED_EDGE('',*,*,#1746,.T.);
#2261=ORIENTED_EDGE('',*,*,#1659,.F.);
#2262=ORIENTED_EDGE('',*,*,#1743,.F.);
#2263=ORIENTED_EDGE('',*,*,#1740,.T.);
#2264=ORIENTED_EDGE('',*,*,#1650,.T.);
#2265=ORIENTED_EDGE('',*,*,#1647,.F.);
#2266=ORIENTED_EDGE('',*,*,#1644,.F.);
#2267=ORIENTED_EDGE('',*,*,#1653,.T.);
#2268=ORIENTED_EDGE('',*,*,#1747,.F.);
#2269=ORIENTED_EDGE('',*,*,#1748,.F.);
#2270=ORIENTED_EDGE('',*,*,#1749,.T.);
#2271=ORIENTED_EDGE('',*,*,#1750,.T.);
#2272=ORIENTED_EDGE('',*,*,#1684,.T.);
#2273=ORIENTED_EDGE('',*,*,#1751,.T.);
#2274=ORIENTED_EDGE('',*,*,#1714,.T.);
#2275=ORIENTED_EDGE('',*,*,#1742,.F.);
#2276=ORIENTED_EDGE('',*,*,#1752,.T.);
#2277=ORIENTED_EDGE('',*,*,#1715,.F.);
#2278=ORIENTED_EDGE('',*,*,#1751,.F.);
#2279=ORIENTED_EDGE('',*,*,#1683,.F.);
#2280=ORIENTED_EDGE('',*,*,#1695,.T.);
#2281=ORIENTED_EDGE('',*,*,#1716,.F.);
#2282=ORIENTED_EDGE('',*,*,#1752,.F.);
#2283=ORIENTED_EDGE('',*,*,#1682,.F.);
#2284=ORIENTED_EDGE('',*,*,#1753,.F.);
#2285=ORIENTED_EDGE('',*,*,#1702,.F.);
#2286=ORIENTED_EDGE('',*,*,#1689,.T.);
#2287=ORIENTED_EDGE('',*,*,#1674,.F.);
#2288=ORIENTED_EDGE('',*,*,#1754,.F.);
#2289=ORIENTED_EDGE('',*,*,#1703,.F.);
#2290=ORIENTED_EDGE('',*,*,#1753,.T.);
#2291=ORIENTED_EDGE('',*,*,#1673,.F.);
#2292=ORIENTED_EDGE('',*,*,#1672,.T.);
#2293=ORIENTED_EDGE('',*,*,#1738,.F.);
#2294=ORIENTED_EDGE('',*,*,#1704,.T.);
#2295=ORIENTED_EDGE('',*,*,#1754,.T.);
#2296=ORIENTED_EDGE('',*,*,#1667,.T.);
#2297=ORIENTED_EDGE('',*,*,#1734,.T.);
#2298=ORIENTED_EDGE('',*,*,#1699,.T.);
#2299=ORIENTED_EDGE('',*,*,#1755,.T.);
#2300=ORIENTED_EDGE('',*,*,#1756,.F.);
#2301=ORIENTED_EDGE('',*,*,#1707,.F.);
#2302=ORIENTED_EDGE('',*,*,#1662,.F.);
#2303=ORIENTED_EDGE('',*,*,#1669,.F.);
#2304=ORIENTED_EDGE('',*,*,#1668,.T.);
#2305=ORIENTED_EDGE('',*,*,#1755,.F.);
#2306=ORIENTED_EDGE('',*,*,#1708,.T.);
#2307=ORIENTED_EDGE('',*,*,#1756,.T.);
#2308=ORIENTED_EDGE('',*,*,#1678,.T.);
#2309=ORIENTED_EDGE('',*,*,#1757,.T.);
#2310=ORIENTED_EDGE('',*,*,#1709,.T.);
#2311=ORIENTED_EDGE('',*,*,#1733,.T.);
#2312=ORIENTED_EDGE('',*,*,#1656,.F.);
#2313=ORIENTED_EDGE('',*,*,#1711,.F.);
#2314=ORIENTED_EDGE('',*,*,#1758,.F.);
#2315=ORIENTED_EDGE('',*,*,#1687,.F.);
#2316=ORIENTED_EDGE('',*,*,#1688,.T.);
#2317=ORIENTED_EDGE('',*,*,#1758,.T.);
#2318=ORIENTED_EDGE('',*,*,#1710,.T.);
#2319=ORIENTED_EDGE('',*,*,#1757,.F.);
#2320=ORIENTED_EDGE('',*,*,#1747,.T.);
#2321=ORIENTED_EDGE('',*,*,#1759,.T.);
#2322=ORIENTED_EDGE('',*,*,#1727,.T.);
#2323=ORIENTED_EDGE('',*,*,#1760,.F.);
#2324=ORIENTED_EDGE('',*,*,#1748,.T.);
#2325=ORIENTED_EDGE('',*,*,#1760,.T.);
#2326=ORIENTED_EDGE('',*,*,#1730,.T.);
#2327=ORIENTED_EDGE('',*,*,#1761,.F.);
#2328=ORIENTED_EDGE('',*,*,#1761,.T.);
#2329=ORIENTED_EDGE('',*,*,#1729,.F.);
#2330=ORIENTED_EDGE('',*,*,#1762,.F.);
#2331=ORIENTED_EDGE('',*,*,#1749,.F.);
#2332=ORIENTED_EDGE('',*,*,#1762,.T.);
#2333=ORIENTED_EDGE('',*,*,#1728,.F.);
#2334=ORIENTED_EDGE('',*,*,#1759,.F.);
#2335=ORIENTED_EDGE('',*,*,#1750,.F.);
#2336=ORIENTED_EDGE('',*,*,#1763,.T.);
#2337=ORIENTED_EDGE('',*,*,#1764,.T.);
#2338=ORIENTED_EDGE('',*,*,#1765,.F.);
#2339=ORIENTED_EDGE('',*,*,#1766,.F.);
#2340=ORIENTED_EDGE('',*,*,#1767,.F.);
#2341=ORIENTED_EDGE('',*,*,#1768,.T.);
#2342=ORIENTED_EDGE('',*,*,#1769,.T.);
#2343=ORIENTED_EDGE('',*,*,#1770,.F.);
#2344=ORIENTED_EDGE('',*,*,#1771,.T.);
#2345=ORIENTED_EDGE('',*,*,#1772,.T.);
#2346=ORIENTED_EDGE('',*,*,#1773,.F.);
#2347=ORIENTED_EDGE('',*,*,#1774,.F.);
#2348=ORIENTED_EDGE('',*,*,#1775,.T.);
#2349=ORIENTED_EDGE('',*,*,#1776,.F.);
#2350=ORIENTED_EDGE('',*,*,#1777,.F.);
#2351=ORIENTED_EDGE('',*,*,#1778,.T.);
#2352=ORIENTED_EDGE('',*,*,#1779,.T.);
#2353=ORIENTED_EDGE('',*,*,#1780,.T.);
#2354=ORIENTED_EDGE('',*,*,#1781,.F.);
#2355=ORIENTED_EDGE('',*,*,#1782,.F.);
#2356=ORIENTED_EDGE('',*,*,#1783,.F.);
#2357=ORIENTED_EDGE('',*,*,#1784,.T.);
#2358=ORIENTED_EDGE('',*,*,#1785,.T.);
#2359=ORIENTED_EDGE('',*,*,#1786,.F.);
#2360=ORIENTED_EDGE('',*,*,#1787,.F.);
#2361=ORIENTED_EDGE('',*,*,#1788,.T.);
#2362=ORIENTED_EDGE('',*,*,#1789,.T.);
#2363=ORIENTED_EDGE('',*,*,#1790,.T.);
#2364=ORIENTED_EDGE('',*,*,#1789,.F.);
#2365=ORIENTED_EDGE('',*,*,#1791,.T.);
#2366=ORIENTED_EDGE('',*,*,#1792,.T.);
#2367=ORIENTED_EDGE('',*,*,#1793,.T.);
#2368=ORIENTED_EDGE('',*,*,#1792,.F.);
#2369=ORIENTED_EDGE('',*,*,#1794,.T.);
#2370=ORIENTED_EDGE('',*,*,#1795,.T.);
#2371=ORIENTED_EDGE('',*,*,#1796,.T.);
#2372=ORIENTED_EDGE('',*,*,#1795,.F.);
#2373=ORIENTED_EDGE('',*,*,#1797,.T.);
#2374=ORIENTED_EDGE('',*,*,#1787,.T.);
#2375=ORIENTED_EDGE('',*,*,#1798,.T.);
#2376=ORIENTED_EDGE('',*,*,#1799,.F.);
#2377=ORIENTED_EDGE('',*,*,#1800,.T.);
#2378=ORIENTED_EDGE('',*,*,#1801,.T.);
#2379=ORIENTED_EDGE('',*,*,#1802,.T.);
#2380=ORIENTED_EDGE('',*,*,#1803,.F.);
#2381=ORIENTED_EDGE('',*,*,#1804,.T.);
#2382=ORIENTED_EDGE('',*,*,#1805,.F.);
#2383=ORIENTED_EDGE('',*,*,#1801,.F.);
#2384=ORIENTED_EDGE('',*,*,#1806,.F.);
#2385=ORIENTED_EDGE('',*,*,#1807,.T.);
#2386=ORIENTED_EDGE('',*,*,#1808,.F.);
#2387=ORIENTED_EDGE('',*,*,#1804,.F.);
#2388=ORIENTED_EDGE('',*,*,#1807,.F.);
#2389=ORIENTED_EDGE('',*,*,#1809,.T.);
#2390=ORIENTED_EDGE('',*,*,#1799,.T.);
#2391=ORIENTED_EDGE('',*,*,#1810,.T.);
#2392=ORIENTED_EDGE('',*,*,#1811,.T.);
#2393=ORIENTED_EDGE('',*,*,#1812,.F.);
#2394=ORIENTED_EDGE('',*,*,#1813,.F.);
#2395=ORIENTED_EDGE('',*,*,#1814,.T.);
#2396=ORIENTED_EDGE('',*,*,#1815,.T.);
#2397=ORIENTED_EDGE('',*,*,#1816,.T.);
#2398=ORIENTED_EDGE('',*,*,#1817,.T.);
#2399=ORIENTED_EDGE('',*,*,#1818,.T.);
#2400=ORIENTED_EDGE('',*,*,#1819,.F.);
#2401=ORIENTED_EDGE('',*,*,#1820,.T.);
#2402=ORIENTED_EDGE('',*,*,#1821,.T.);
#2403=ORIENTED_EDGE('',*,*,#1822,.F.);
#2404=ORIENTED_EDGE('',*,*,#1806,.T.);
#2405=ORIENTED_EDGE('',*,*,#1803,.T.);
#2406=ORIENTED_EDGE('',*,*,#1800,.F.);
#2407=ORIENTED_EDGE('',*,*,#1809,.F.);
#2408=ORIENTED_EDGE('',*,*,#1794,.F.);
#2409=ORIENTED_EDGE('',*,*,#1791,.F.);
#2410=ORIENTED_EDGE('',*,*,#1788,.F.);
#2411=ORIENTED_EDGE('',*,*,#1797,.F.);
#2412=ORIENTED_EDGE('',*,*,#1823,.T.);
#2413=ORIENTED_EDGE('',*,*,#1824,.F.);
#2414=ORIENTED_EDGE('',*,*,#1825,.F.);
#2415=ORIENTED_EDGE('',*,*,#1826,.T.);
#2416=ORIENTED_EDGE('',*,*,#1827,.T.);
#2417=ORIENTED_EDGE('',*,*,#1828,.T.);
#2418=ORIENTED_EDGE('',*,*,#1829,.T.);
#2419=ORIENTED_EDGE('',*,*,#1830,.T.);
#2420=ORIENTED_EDGE('',*,*,#1831,.T.);
#2421=ORIENTED_EDGE('',*,*,#1832,.T.);
#2422=ORIENTED_EDGE('',*,*,#1833,.F.);
#2423=ORIENTED_EDGE('',*,*,#1834,.F.);
#2424=ORIENTED_EDGE('',*,*,#1802,.F.);
#2425=ORIENTED_EDGE('',*,*,#1805,.T.);
#2426=ORIENTED_EDGE('',*,*,#1808,.T.);
#2427=ORIENTED_EDGE('',*,*,#1810,.F.);
#2428=ORIENTED_EDGE('',*,*,#1790,.F.);
#2429=ORIENTED_EDGE('',*,*,#1793,.F.);
#2430=ORIENTED_EDGE('',*,*,#1796,.F.);
#2431=ORIENTED_EDGE('',*,*,#1798,.F.);
#2432=ORIENTED_EDGE('',*,*,#1835,.F.);
#2433=ORIENTED_EDGE('',*,*,#1836,.F.);
#2434=ORIENTED_EDGE('',*,*,#1837,.T.);
#2435=ORIENTED_EDGE('',*,*,#1838,.T.);
#2436=ORIENTED_EDGE('',*,*,#1836,.T.);
#2437=ORIENTED_EDGE('',*,*,#1839,.F.);
#2438=ORIENTED_EDGE('',*,*,#1823,.F.);
#2439=ORIENTED_EDGE('',*,*,#1840,.T.);
#2440=ORIENTED_EDGE('',*,*,#1825,.T.);
#2441=ORIENTED_EDGE('',*,*,#1841,.F.);
#2442=ORIENTED_EDGE('',*,*,#1842,.F.);
#2443=ORIENTED_EDGE('',*,*,#1843,.T.);
#2444=ORIENTED_EDGE('',*,*,#1842,.T.);
#2445=ORIENTED_EDGE('',*,*,#1844,.F.);
#2446=ORIENTED_EDGE('',*,*,#1845,.F.);
#2447=ORIENTED_EDGE('',*,*,#1846,.T.);
#2448=ORIENTED_EDGE('',*,*,#1845,.T.);
#2449=ORIENTED_EDGE('',*,*,#1847,.F.);
#2450=ORIENTED_EDGE('',*,*,#1775,.F.);
#2451=ORIENTED_EDGE('',*,*,#1848,.T.);
#2452=ORIENTED_EDGE('',*,*,#1777,.T.);
#2453=ORIENTED_EDGE('',*,*,#1849,.F.);
#2454=ORIENTED_EDGE('',*,*,#1838,.F.);
#2455=ORIENTED_EDGE('',*,*,#1850,.T.);
#2456=ORIENTED_EDGE('',*,*,#1776,.T.);
#2457=ORIENTED_EDGE('',*,*,#1847,.T.);
#2458=ORIENTED_EDGE('',*,*,#1844,.T.);
#2459=ORIENTED_EDGE('',*,*,#1841,.T.);
#2460=ORIENTED_EDGE('',*,*,#1824,.T.);
#2461=ORIENTED_EDGE('',*,*,#1839,.T.);
#2462=ORIENTED_EDGE('',*,*,#1835,.T.);
#2463=ORIENTED_EDGE('',*,*,#1849,.T.);
#2464=ORIENTED_EDGE('',*,*,#1851,.F.);
#2465=ORIENTED_EDGE('',*,*,#1764,.F.);
#2466=ORIENTED_EDGE('',*,*,#1852,.F.);
#2467=ORIENTED_EDGE('',*,*,#1853,.F.);
#2468=ORIENTED_EDGE('',*,*,#1854,.F.);
#2469=ORIENTED_EDGE('',*,*,#1812,.T.);
#2470=ORIENTED_EDGE('',*,*,#1855,.F.);
#2471=ORIENTED_EDGE('',*,*,#1856,.T.);
#2472=ORIENTED_EDGE('',*,*,#1778,.F.);
#2473=ORIENTED_EDGE('',*,*,#1850,.F.);
#2474=ORIENTED_EDGE('',*,*,#1837,.F.);
#2475=ORIENTED_EDGE('',*,*,#1840,.F.);
#2476=ORIENTED_EDGE('',*,*,#1826,.F.);
#2477=ORIENTED_EDGE('',*,*,#1843,.F.);
#2478=ORIENTED_EDGE('',*,*,#1846,.F.);
#2479=ORIENTED_EDGE('',*,*,#1848,.F.);
#2480=ORIENTED_EDGE('',*,*,#1857,.T.);
#2481=ORIENTED_EDGE('',*,*,#1858,.F.);
#2482=ORIENTED_EDGE('',*,*,#1859,.T.);
#2483=ORIENTED_EDGE('',*,*,#1814,.F.);
#2484=ORIENTED_EDGE('',*,*,#1860,.T.);
#2485=ORIENTED_EDGE('',*,*,#1861,.T.);
#2486=ORIENTED_EDGE('',*,*,#1862,.T.);
#2487=ORIENTED_EDGE('',*,*,#1766,.T.);
#2488=ORIENTED_EDGE('',*,*,#1855,.T.);
#2489=ORIENTED_EDGE('',*,*,#1811,.F.);
#2490=ORIENTED_EDGE('',*,*,#1859,.F.);
#2491=ORIENTED_EDGE('',*,*,#1863,.T.);
#2492=ORIENTED_EDGE('',*,*,#1813,.T.);
#2493=ORIENTED_EDGE('',*,*,#1854,.T.);
#2494=ORIENTED_EDGE('',*,*,#1864,.F.);
#2495=ORIENTED_EDGE('',*,*,#1860,.F.);
#2496=ORIENTED_EDGE('',*,*,#1864,.T.);
#2497=ORIENTED_EDGE('',*,*,#1853,.T.);
#2498=ORIENTED_EDGE('',*,*,#1865,.F.);
#2499=ORIENTED_EDGE('',*,*,#1861,.F.);
#2500=ORIENTED_EDGE('',*,*,#1865,.T.);
#2501=ORIENTED_EDGE('',*,*,#1852,.T.);
#2502=ORIENTED_EDGE('',*,*,#1763,.F.);
#2503=ORIENTED_EDGE('',*,*,#1862,.F.);
#2504=ORIENTED_EDGE('',*,*,#1765,.T.);
#2505=ORIENTED_EDGE('',*,*,#1851,.T.);
#2506=ORIENTED_EDGE('',*,*,#1866,.F.);
#2507=ORIENTED_EDGE('',*,*,#1857,.F.);
#2508=ORIENTED_EDGE('',*,*,#1866,.T.);
#2509=ORIENTED_EDGE('',*,*,#1856,.F.);
#2510=ORIENTED_EDGE('',*,*,#1863,.F.);
#2511=ORIENTED_EDGE('',*,*,#1858,.T.);
#2512=ORIENTED_EDGE('',*,*,#1867,.T.);
#2513=ORIENTED_EDGE('',*,*,#1828,.F.);
#2514=ORIENTED_EDGE('',*,*,#1868,.F.);
#2515=ORIENTED_EDGE('',*,*,#1816,.F.);
#2516=ORIENTED_EDGE('',*,*,#1868,.T.);
#2517=ORIENTED_EDGE('',*,*,#1827,.F.);
#2518=ORIENTED_EDGE('',*,*,#1869,.F.);
#2519=ORIENTED_EDGE('',*,*,#1817,.F.);
#2520=ORIENTED_EDGE('',*,*,#1869,.T.);
#2521=ORIENTED_EDGE('',*,*,#1830,.F.);
#2522=ORIENTED_EDGE('',*,*,#1870,.F.);
#2523=ORIENTED_EDGE('',*,*,#1818,.F.);
#2524=ORIENTED_EDGE('',*,*,#1870,.T.);
#2525=ORIENTED_EDGE('',*,*,#1829,.F.);
#2526=ORIENTED_EDGE('',*,*,#1867,.F.);
#2527=ORIENTED_EDGE('',*,*,#1815,.F.);
#2528=ORIENTED_EDGE('',*,*,#1871,.T.);
#2529=ORIENTED_EDGE('',*,*,#1832,.F.);
#2530=ORIENTED_EDGE('',*,*,#1872,.F.);
#2531=ORIENTED_EDGE('',*,*,#1820,.F.);
#2532=ORIENTED_EDGE('',*,*,#1872,.T.);
#2533=ORIENTED_EDGE('',*,*,#1831,.F.);
#2534=ORIENTED_EDGE('',*,*,#1873,.F.);
#2535=ORIENTED_EDGE('',*,*,#1821,.F.);
#2536=ORIENTED_EDGE('',*,*,#1822,.T.);
#2537=ORIENTED_EDGE('',*,*,#1873,.T.);
#2538=ORIENTED_EDGE('',*,*,#1834,.T.);
#2539=ORIENTED_EDGE('',*,*,#1874,.F.);
#2540=ORIENTED_EDGE('',*,*,#1819,.T.);
#2541=ORIENTED_EDGE('',*,*,#1874,.T.);
#2542=ORIENTED_EDGE('',*,*,#1833,.T.);
#2543=ORIENTED_EDGE('',*,*,#1871,.F.);
#2544=ORIENTED_EDGE('',*,*,#1875,.T.);
#2545=ORIENTED_EDGE('',*,*,#1780,.F.);
#2546=ORIENTED_EDGE('',*,*,#1876,.F.);
#2547=ORIENTED_EDGE('',*,*,#1768,.F.);
#2548=ORIENTED_EDGE('',*,*,#1876,.T.);
#2549=ORIENTED_EDGE('',*,*,#1779,.F.);
#2550=ORIENTED_EDGE('',*,*,#1877,.F.);
#2551=ORIENTED_EDGE('',*,*,#1769,.F.);
#2552=ORIENTED_EDGE('',*,*,#1770,.T.);
#2553=ORIENTED_EDGE('',*,*,#1877,.T.);
#2554=ORIENTED_EDGE('',*,*,#1782,.T.);
#2555=ORIENTED_EDGE('',*,*,#1878,.F.);
#2556=ORIENTED_EDGE('',*,*,#1767,.T.);
#2557=ORIENTED_EDGE('',*,*,#1878,.T.);
#2558=ORIENTED_EDGE('',*,*,#1781,.T.);
#2559=ORIENTED_EDGE('',*,*,#1875,.F.);
#2560=ORIENTED_EDGE('',*,*,#1879,.T.);
#2561=ORIENTED_EDGE('',*,*,#1784,.F.);
#2562=ORIENTED_EDGE('',*,*,#1880,.F.);
#2563=ORIENTED_EDGE('',*,*,#1772,.F.);
#2564=ORIENTED_EDGE('',*,*,#1773,.T.);
#2565=ORIENTED_EDGE('',*,*,#1880,.T.);
#2566=ORIENTED_EDGE('',*,*,#1783,.T.);
#2567=ORIENTED_EDGE('',*,*,#1881,.F.);
#2568=ORIENTED_EDGE('',*,*,#1774,.T.);
#2569=ORIENTED_EDGE('',*,*,#1881,.T.);
#2570=ORIENTED_EDGE('',*,*,#1786,.T.);
#2571=ORIENTED_EDGE('',*,*,#1882,.F.);
#2572=ORIENTED_EDGE('',*,*,#1882,.T.);
#2573=ORIENTED_EDGE('',*,*,#1785,.F.);
#2574=ORIENTED_EDGE('',*,*,#1879,.F.);
#2575=ORIENTED_EDGE('',*,*,#1771,.F.);
#2576=ORIENTED_EDGE('',*,*,#1883,.F.);
#2577=ORIENTED_EDGE('',*,*,#1884,.T.);
#2578=ORIENTED_EDGE('',*,*,#1885,.T.);
#2579=ORIENTED_EDGE('',*,*,#1884,.F.);
#2580=ORIENTED_EDGE('',*,*,#1886,.T.);
#2581=ORIENTED_EDGE('',*,*,#1885,.F.);
#2582=ORIENTED_EDGE('',*,*,#1886,.F.);
#2583=ORIENTED_EDGE('',*,*,#1887,.T.);
#2584=ORIENTED_EDGE('',*,*,#1888,.T.);
#2585=ORIENTED_EDGE('',*,*,#1887,.F.);
#2586=ORIENTED_EDGE('',*,*,#1888,.F.);
#2587=ORIENTED_EDGE('',*,*,#1889,.T.);
#2588=ORIENTED_EDGE('',*,*,#1889,.F.);
#2589=ORIENTED_EDGE('',*,*,#1890,.T.);
#2590=ORIENTED_EDGE('',*,*,#1891,.T.);
#2591=ORIENTED_EDGE('',*,*,#1890,.F.);
#2592=ORIENTED_EDGE('',*,*,#1892,.T.);
#2593=ORIENTED_EDGE('',*,*,#1891,.F.);
#2594=ORIENTED_EDGE('',*,*,#1892,.F.);
#2595=ORIENTED_EDGE('',*,*,#1893,.T.);
#2596=ORIENTED_EDGE('',*,*,#1894,.T.);
#2597=ORIENTED_EDGE('',*,*,#1893,.F.);
#2598=ORIENTED_EDGE('',*,*,#1894,.F.);
#2599=ORIENTED_EDGE('',*,*,#1883,.T.);
#2600=ORIENTED_EDGE('',*,*,#1895,.T.);
#2601=ORIENTED_EDGE('',*,*,#1896,.F.);
#2602=ORIENTED_EDGE('',*,*,#1897,.T.);
#2603=ORIENTED_EDGE('',*,*,#1895,.F.);
#2604=ORIENTED_EDGE('',*,*,#1897,.F.);
#2605=ORIENTED_EDGE('',*,*,#1896,.T.);
#2606=ORIENTED_EDGE('',*,*,#1898,.T.);
#2607=ORIENTED_EDGE('',*,*,#1899,.T.);
#2608=ORIENTED_EDGE('',*,*,#1900,.F.);
#2609=ORIENTED_EDGE('',*,*,#1901,.F.);
#2610=ORIENTED_EDGE('',*,*,#1902,.F.);
#2611=ORIENTED_EDGE('',*,*,#1903,.F.);
#2612=ORIENTED_EDGE('',*,*,#1904,.T.);
#2613=ORIENTED_EDGE('',*,*,#1905,.T.);
#2614=ORIENTED_EDGE('',*,*,#1906,.T.);
#2615=ORIENTED_EDGE('',*,*,#1907,.T.);
#2616=ORIENTED_EDGE('',*,*,#1908,.T.);
#2617=ORIENTED_EDGE('',*,*,#1909,.T.);
#2618=ORIENTED_EDGE('',*,*,#1910,.T.);
#2619=ORIENTED_EDGE('',*,*,#1911,.T.);
#2620=ORIENTED_EDGE('',*,*,#1912,.T.);
#2621=ORIENTED_EDGE('',*,*,#1913,.T.);
#2622=ORIENTED_EDGE('',*,*,#1914,.T.);
#2623=ORIENTED_EDGE('',*,*,#1915,.F.);
#2624=ORIENTED_EDGE('',*,*,#1916,.F.);
#2625=ORIENTED_EDGE('',*,*,#1917,.F.);
#2626=ORIENTED_EDGE('',*,*,#1918,.T.);
#2627=ORIENTED_EDGE('',*,*,#1919,.F.);
#2628=ORIENTED_EDGE('',*,*,#1920,.T.);
#2629=ORIENTED_EDGE('',*,*,#1921,.F.);
#2630=ORIENTED_EDGE('',*,*,#1922,.F.);
#2631=ORIENTED_EDGE('',*,*,#1923,.T.);
#2632=ORIENTED_EDGE('',*,*,#1924,.F.);
#2633=ORIENTED_EDGE('',*,*,#1912,.F.);
#2634=ORIENTED_EDGE('',*,*,#1925,.T.);
#2635=ORIENTED_EDGE('',*,*,#1926,.T.);
#2636=ORIENTED_EDGE('',*,*,#1927,.F.);
#2637=ORIENTED_EDGE('',*,*,#1928,.F.);
#2638=ORIENTED_EDGE('',*,*,#1927,.T.);
#2639=ORIENTED_EDGE('',*,*,#1929,.T.);
#2640=ORIENTED_EDGE('',*,*,#1930,.F.);
#2641=ORIENTED_EDGE('',*,*,#1931,.F.);
#2642=ORIENTED_EDGE('',*,*,#1930,.T.);
#2643=ORIENTED_EDGE('',*,*,#1932,.T.);
#2644=ORIENTED_EDGE('',*,*,#1933,.F.);
#2645=ORIENTED_EDGE('',*,*,#1934,.T.);
#2646=ORIENTED_EDGE('',*,*,#1935,.T.);
#2647=ORIENTED_EDGE('',*,*,#1936,.F.);
#2648=ORIENTED_EDGE('',*,*,#1937,.F.);
#2649=ORIENTED_EDGE('',*,*,#1905,.F.);
#2650=ORIENTED_EDGE('',*,*,#1938,.F.);
#2651=ORIENTED_EDGE('',*,*,#1939,.T.);
#2652=ORIENTED_EDGE('',*,*,#1940,.T.);
#2653=ORIENTED_EDGE('',*,*,#1914,.F.);
#2654=ORIENTED_EDGE('',*,*,#1941,.T.);
#2655=ORIENTED_EDGE('',*,*,#1942,.T.);
#2656=ORIENTED_EDGE('',*,*,#1943,.F.);
#2657=ORIENTED_EDGE('',*,*,#1944,.F.);
#2658=ORIENTED_EDGE('',*,*,#1945,.F.);
#2659=ORIENTED_EDGE('',*,*,#1906,.F.);
#2660=ORIENTED_EDGE('',*,*,#1937,.T.);
#2661=ORIENTED_EDGE('',*,*,#1946,.F.);
#2662=ORIENTED_EDGE('',*,*,#1947,.F.);
#2663=ORIENTED_EDGE('',*,*,#1899,.F.);
#2664=ORIENTED_EDGE('',*,*,#1948,.F.);
#2665=ORIENTED_EDGE('',*,*,#1949,.T.);
#2666=ORIENTED_EDGE('',*,*,#1950,.T.);
#2667=ORIENTED_EDGE('',*,*,#1920,.F.);
#2668=ORIENTED_EDGE('',*,*,#1951,.T.);
#2669=ORIENTED_EDGE('',*,*,#1952,.T.);
#2670=ORIENTED_EDGE('',*,*,#1953,.F.);
#2671=ORIENTED_EDGE('',*,*,#1900,.T.);
#2672=ORIENTED_EDGE('',*,*,#1947,.T.);
#2673=ORIENTED_EDGE('',*,*,#1954,.F.);
#2674=ORIENTED_EDGE('',*,*,#1955,.F.);
#2675=ORIENTED_EDGE('',*,*,#1901,.T.);
#2676=ORIENTED_EDGE('',*,*,#1953,.T.);
#2677=ORIENTED_EDGE('',*,*,#1956,.F.);
#2678=ORIENTED_EDGE('',*,*,#1957,.F.);
#2679=ORIENTED_EDGE('',*,*,#1902,.T.);
#2680=ORIENTED_EDGE('',*,*,#1955,.T.);
#2681=ORIENTED_EDGE('',*,*,#1958,.F.);
#2682=ORIENTED_EDGE('',*,*,#1959,.F.);
#2683=ORIENTED_EDGE('',*,*,#1916,.T.);
#2684=ORIENTED_EDGE('',*,*,#1960,.F.);
#2685=ORIENTED_EDGE('',*,*,#1961,.F.);
#2686=ORIENTED_EDGE('',*,*,#1962,.T.);
#2687=ORIENTED_EDGE('',*,*,#1903,.T.);
#2688=ORIENTED_EDGE('',*,*,#1957,.T.);
#2689=ORIENTED_EDGE('',*,*,#1963,.F.);
#2690=ORIENTED_EDGE('',*,*,#1964,.F.);
#2691=ORIENTED_EDGE('',*,*,#1917,.T.);
#2692=ORIENTED_EDGE('',*,*,#1959,.T.);
#2693=ORIENTED_EDGE('',*,*,#1965,.F.);
#2694=ORIENTED_EDGE('',*,*,#1966,.F.);
#2695=ORIENTED_EDGE('',*,*,#1918,.F.);
#2696=ORIENTED_EDGE('',*,*,#1964,.T.);
#2697=ORIENTED_EDGE('',*,*,#1967,.T.);
#2698=ORIENTED_EDGE('',*,*,#1968,.F.);
#2699=ORIENTED_EDGE('',*,*,#1951,.F.);
#2700=ORIENTED_EDGE('',*,*,#1919,.T.);
#2701=ORIENTED_EDGE('',*,*,#1966,.T.);
#2702=ORIENTED_EDGE('',*,*,#1969,.F.);
#2703=ORIENTED_EDGE('',*,*,#1970,.F.);
#2704=ORIENTED_EDGE('',*,*,#1932,.F.);
#2705=ORIENTED_EDGE('',*,*,#1929,.F.);
#2706=ORIENTED_EDGE('',*,*,#1926,.F.);
#2707=ORIENTED_EDGE('',*,*,#1971,.F.);
#2708=ORIENTED_EDGE('',*,*,#1972,.F.);
#2709=ORIENTED_EDGE('',*,*,#1973,.F.);
#2710=ORIENTED_EDGE('',*,*,#1954,.T.);
#2711=ORIENTED_EDGE('',*,*,#1952,.F.);
#2712=ORIENTED_EDGE('',*,*,#1968,.T.);
#2713=ORIENTED_EDGE('',*,*,#1967,.F.);
#2714=ORIENTED_EDGE('',*,*,#1965,.T.);
#2715=ORIENTED_EDGE('',*,*,#1963,.T.);
#2716=ORIENTED_EDGE('',*,*,#1958,.T.);
#2717=ORIENTED_EDGE('',*,*,#1956,.T.);
#2718=ORIENTED_EDGE('',*,*,#1974,.T.);
#2719=ORIENTED_EDGE('',*,*,#1933,.T.);
#2720=ORIENTED_EDGE('',*,*,#1970,.T.);
#2721=ORIENTED_EDGE('',*,*,#1975,.F.);
#2722=ORIENTED_EDGE('',*,*,#1976,.T.);
#2723=ORIENTED_EDGE('',*,*,#1975,.T.);
#2724=ORIENTED_EDGE('',*,*,#1969,.T.);
#2725=ORIENTED_EDGE('',*,*,#1977,.F.);
#2726=ORIENTED_EDGE('',*,*,#1907,.F.);
#2727=ORIENTED_EDGE('',*,*,#1945,.T.);
#2728=ORIENTED_EDGE('',*,*,#1978,.F.);
#2729=ORIENTED_EDGE('',*,*,#1979,.T.);
#2730=ORIENTED_EDGE('',*,*,#1980,.F.);
#2731=ORIENTED_EDGE('',*,*,#1908,.F.);
#2732=ORIENTED_EDGE('',*,*,#1977,.T.);
#2733=ORIENTED_EDGE('',*,*,#1973,.T.);
#2734=ORIENTED_EDGE('',*,*,#1981,.F.);
#2735=ORIENTED_EDGE('',*,*,#1910,.F.);
#2736=ORIENTED_EDGE('',*,*,#1982,.F.);
#2737=ORIENTED_EDGE('',*,*,#1983,.F.);
#2738=ORIENTED_EDGE('',*,*,#1984,.T.);
#2739=ORIENTED_EDGE('',*,*,#1909,.F.);
#2740=ORIENTED_EDGE('',*,*,#1980,.T.);
#2741=ORIENTED_EDGE('',*,*,#1972,.T.);
#2742=ORIENTED_EDGE('',*,*,#1925,.F.);
#2743=ORIENTED_EDGE('',*,*,#1911,.F.);
#2744=ORIENTED_EDGE('',*,*,#1981,.T.);
#2745=ORIENTED_EDGE('',*,*,#1971,.T.);
#2746=ORIENTED_EDGE('',*,*,#1985,.T.);
#2747=ORIENTED_EDGE('',*,*,#1941,.F.);
#2748=ORIENTED_EDGE('',*,*,#1913,.F.);
#2749=ORIENTED_EDGE('',*,*,#1924,.T.);
#2750=ORIENTED_EDGE('',*,*,#1974,.F.);
#2751=ORIENTED_EDGE('',*,*,#1976,.F.);
#2752=ORIENTED_EDGE('',*,*,#1986,.F.);
#2753=ORIENTED_EDGE('',*,*,#1987,.T.);
#2754=ORIENTED_EDGE('',*,*,#1934,.F.);
#2755=ORIENTED_EDGE('',*,*,#1979,.F.);
#2756=ORIENTED_EDGE('',*,*,#1988,.F.);
#2757=ORIENTED_EDGE('',*,*,#1989,.T.);
#2758=ORIENTED_EDGE('',*,*,#1986,.T.);
#2759=ORIENTED_EDGE('',*,*,#1978,.T.);
#2760=ORIENTED_EDGE('',*,*,#1946,.T.);
#2761=ORIENTED_EDGE('',*,*,#1936,.T.);
#2762=ORIENTED_EDGE('',*,*,#1990,.F.);
#2763=ORIENTED_EDGE('',*,*,#1988,.T.);
#2764=ORIENTED_EDGE('',*,*,#1935,.F.);
#2765=ORIENTED_EDGE('',*,*,#1987,.F.);
#2766=ORIENTED_EDGE('',*,*,#1989,.F.);
#2767=ORIENTED_EDGE('',*,*,#1990,.T.);
#2768=ORIENTED_EDGE('',*,*,#1928,.T.);
#2769=ORIENTED_EDGE('',*,*,#1931,.T.);
#2770=ORIENTED_EDGE('',*,*,#1944,.T.);
#2771=ORIENTED_EDGE('',*,*,#1991,.F.);
#2772=ORIENTED_EDGE('',*,*,#1992,.T.);
#2773=ORIENTED_EDGE('',*,*,#1922,.T.);
#2774=ORIENTED_EDGE('',*,*,#1992,.F.);
#2775=ORIENTED_EDGE('',*,*,#1993,.F.);
#2776=ORIENTED_EDGE('',*,*,#1994,.T.);
#2777=ORIENTED_EDGE('',*,*,#1985,.F.);
#2778=ORIENTED_EDGE('',*,*,#1923,.F.);
#2779=ORIENTED_EDGE('',*,*,#1994,.F.);
#2780=ORIENTED_EDGE('',*,*,#1995,.T.);
#2781=ORIENTED_EDGE('',*,*,#1942,.F.);
#2782=ORIENTED_EDGE('',*,*,#1991,.T.);
#2783=ORIENTED_EDGE('',*,*,#1943,.T.);
#2784=ORIENTED_EDGE('',*,*,#1995,.F.);
#2785=ORIENTED_EDGE('',*,*,#1993,.T.);
#2786=ORIENTED_EDGE('',*,*,#1904,.F.);
#2787=ORIENTED_EDGE('',*,*,#1962,.F.);
#2788=ORIENTED_EDGE('',*,*,#1996,.T.);
#2789=ORIENTED_EDGE('',*,*,#1938,.T.);
#2790=ORIENTED_EDGE('',*,*,#1915,.T.);
#2791=ORIENTED_EDGE('',*,*,#1940,.F.);
#2792=ORIENTED_EDGE('',*,*,#1997,.F.);
#2793=ORIENTED_EDGE('',*,*,#1960,.T.);
#2794=ORIENTED_EDGE('',*,*,#1996,.F.);
#2795=ORIENTED_EDGE('',*,*,#1961,.T.);
#2796=ORIENTED_EDGE('',*,*,#1997,.T.);
#2797=ORIENTED_EDGE('',*,*,#1939,.F.);
#2798=ORIENTED_EDGE('',*,*,#1898,.F.);
#2799=ORIENTED_EDGE('',*,*,#1984,.F.);
#2800=ORIENTED_EDGE('',*,*,#1998,.T.);
#2801=ORIENTED_EDGE('',*,*,#1948,.T.);
#2802=ORIENTED_EDGE('',*,*,#1921,.T.);
#2803=ORIENTED_EDGE('',*,*,#1950,.F.);
#2804=ORIENTED_EDGE('',*,*,#1999,.F.);
#2805=ORIENTED_EDGE('',*,*,#1982,.T.);
#2806=ORIENTED_EDGE('',*,*,#1998,.F.);
#2807=ORIENTED_EDGE('',*,*,#1983,.T.);
#2808=ORIENTED_EDGE('',*,*,#1999,.T.);
#2809=ORIENTED_EDGE('',*,*,#1949,.F.);
#2810=ORIENTED_EDGE('',*,*,#2000,.T.);
#2811=ORIENTED_EDGE('',*,*,#2001,.F.);
#2812=ORIENTED_EDGE('',*,*,#2002,.F.);
#2813=ORIENTED_EDGE('',*,*,#2003,.T.);
#2814=ORIENTED_EDGE('',*,*,#2004,.F.);
#2815=ORIENTED_EDGE('',*,*,#2005,.T.);
#2816=ORIENTED_EDGE('',*,*,#2006,.T.);
#2817=ORIENTED_EDGE('',*,*,#2007,.F.);
#2818=ORIENTED_EDGE('',*,*,#2008,.F.);
#2819=ORIENTED_EDGE('',*,*,#2009,.T.);
#2820=ORIENTED_EDGE('',*,*,#2010,.T.);
#2821=ORIENTED_EDGE('',*,*,#2000,.F.);
#2822=ORIENTED_EDGE('',*,*,#2011,.F.);
#2823=ORIENTED_EDGE('',*,*,#2012,.F.);
#2824=ORIENTED_EDGE('',*,*,#2013,.T.);
#2825=ORIENTED_EDGE('',*,*,#2002,.T.);
#2826=ORIENTED_EDGE('',*,*,#2014,.F.);
#2827=ORIENTED_EDGE('',*,*,#2015,.T.);
#2828=ORIENTED_EDGE('',*,*,#2016,.T.);
#2829=ORIENTED_EDGE('',*,*,#2017,.T.);
#2830=ORIENTED_EDGE('',*,*,#2018,.F.);
#2831=ORIENTED_EDGE('',*,*,#2019,.T.);
#2832=ORIENTED_EDGE('',*,*,#2020,.F.);
#2833=ORIENTED_EDGE('',*,*,#2021,.T.);
#2834=ORIENTED_EDGE('',*,*,#2022,.F.);
#2835=ORIENTED_EDGE('',*,*,#2023,.F.);
#2836=ORIENTED_EDGE('',*,*,#2024,.F.);
#2837=ORIENTED_EDGE('',*,*,#2025,.T.);
#2838=ORIENTED_EDGE('',*,*,#2026,.T.);
#2839=ORIENTED_EDGE('',*,*,#2008,.T.);
#2840=ORIENTED_EDGE('',*,*,#2003,.F.);
#2841=ORIENTED_EDGE('',*,*,#2013,.F.);
#2842=ORIENTED_EDGE('',*,*,#2027,.T.);
#2843=ORIENTED_EDGE('',*,*,#2021,.F.);
#2844=ORIENTED_EDGE('',*,*,#2028,.T.);
#2845=ORIENTED_EDGE('',*,*,#2018,.T.);
#2846=ORIENTED_EDGE('',*,*,#2010,.F.);
#2847=ORIENTED_EDGE('',*,*,#2029,.F.);
#2848=ORIENTED_EDGE('',*,*,#2016,.F.);
#2849=ORIENTED_EDGE('',*,*,#2030,.F.);
#2850=ORIENTED_EDGE('',*,*,#2023,.T.);
#2851=ORIENTED_EDGE('',*,*,#2031,.F.);
#2852=ORIENTED_EDGE('',*,*,#2014,.T.);
#2853=ORIENTED_EDGE('',*,*,#2001,.T.);
#2854=ORIENTED_EDGE('',*,*,#2024,.T.);
#2855=ORIENTED_EDGE('',*,*,#2030,.T.);
#2856=ORIENTED_EDGE('',*,*,#2019,.F.);
#2857=ORIENTED_EDGE('',*,*,#2028,.F.);
#2858=ORIENTED_EDGE('',*,*,#2015,.F.);
#2859=ORIENTED_EDGE('',*,*,#2032,.T.);
#2860=ORIENTED_EDGE('',*,*,#2025,.F.);
#2861=ORIENTED_EDGE('',*,*,#2032,.F.);
#2862=ORIENTED_EDGE('',*,*,#2020,.T.);
#2863=ORIENTED_EDGE('',*,*,#2033,.T.);
#2864=ORIENTED_EDGE('',*,*,#2011,.T.);
#2865=ORIENTED_EDGE('',*,*,#2033,.F.);
#2866=ORIENTED_EDGE('',*,*,#2012,.T.);
#2867=ORIENTED_EDGE('',*,*,#2031,.T.);
#2868=ORIENTED_EDGE('',*,*,#2022,.T.);
#2869=ORIENTED_EDGE('',*,*,#2027,.F.);
#2870=ORIENTED_EDGE('',*,*,#2017,.F.);
#2871=ORIENTED_EDGE('',*,*,#2029,.T.);
#2872=ORIENTED_EDGE('',*,*,#2009,.F.);
#2873=ORIENTED_EDGE('',*,*,#2026,.F.);
#2874=ORIENTED_EDGE('',*,*,#2004,.T.);
#2875=ORIENTED_EDGE('',*,*,#2034,.F.);
#2876=ORIENTED_EDGE('',*,*,#2035,.F.);
#2877=ORIENTED_EDGE('',*,*,#2036,.T.);
#2878=ORIENTED_EDGE('',*,*,#2005,.F.);
#2879=ORIENTED_EDGE('',*,*,#2036,.F.);
#2880=ORIENTED_EDGE('',*,*,#2037,.T.);
#2881=ORIENTED_EDGE('',*,*,#2038,.T.);
#2882=ORIENTED_EDGE('',*,*,#2006,.F.);
#2883=ORIENTED_EDGE('',*,*,#2038,.F.);
#2884=ORIENTED_EDGE('',*,*,#2039,.T.);
#2885=ORIENTED_EDGE('',*,*,#2040,.T.);
#2886=ORIENTED_EDGE('',*,*,#2007,.T.);
#2887=ORIENTED_EDGE('',*,*,#2040,.F.);
#2888=ORIENTED_EDGE('',*,*,#2041,.F.);
#2889=ORIENTED_EDGE('',*,*,#2034,.T.);
#2890=ORIENTED_EDGE('',*,*,#2035,.T.);
#2891=ORIENTED_EDGE('',*,*,#2041,.T.);
#2892=ORIENTED_EDGE('',*,*,#2039,.F.);
#2893=ORIENTED_EDGE('',*,*,#2037,.F.);
#2894=ORIENTED_EDGE('',*,*,#2042,.T.);
#2895=ORIENTED_EDGE('',*,*,#2043,.T.);
#2896=ORIENTED_EDGE('',*,*,#2044,.F.);
#2897=ORIENTED_EDGE('',*,*,#2045,.F.);
#2898=ORIENTED_EDGE('',*,*,#2046,.F.);
#2899=ORIENTED_EDGE('',*,*,#2047,.T.);
#2900=ORIENTED_EDGE('',*,*,#2044,.T.);
#2901=ORIENTED_EDGE('',*,*,#2048,.T.);
#2902=ORIENTED_EDGE('',*,*,#2049,.T.);
#2903=ORIENTED_EDGE('',*,*,#2050,.F.);
#2904=ORIENTED_EDGE('',*,*,#2051,.F.);
#2905=ORIENTED_EDGE('',*,*,#2052,.F.);
#2906=ORIENTED_EDGE('',*,*,#2053,.T.);
#2907=ORIENTED_EDGE('',*,*,#2054,.T.);
#2908=ORIENTED_EDGE('',*,*,#2055,.F.);
#2909=ORIENTED_EDGE('',*,*,#2056,.F.);
#2910=ORIENTED_EDGE('',*,*,#2057,.F.);
#2911=ORIENTED_EDGE('',*,*,#2058,.T.);
#2912=ORIENTED_EDGE('',*,*,#2057,.T.);
#2913=ORIENTED_EDGE('',*,*,#2059,.T.);
#2914=ORIENTED_EDGE('',*,*,#2060,.F.);
#2915=ORIENTED_EDGE('',*,*,#2061,.F.);
#2916=ORIENTED_EDGE('',*,*,#2042,.F.);
#2917=ORIENTED_EDGE('',*,*,#2062,.T.);
#2918=ORIENTED_EDGE('',*,*,#2063,.F.);
#2919=ORIENTED_EDGE('',*,*,#2064,.F.);
#2920=ORIENTED_EDGE('',*,*,#2065,.F.);
#2921=ORIENTED_EDGE('',*,*,#2066,.T.);
#2922=ORIENTED_EDGE('',*,*,#2067,.F.);
#2923=ORIENTED_EDGE('',*,*,#2068,.F.);
#2924=ORIENTED_EDGE('',*,*,#2060,.T.);
#2925=ORIENTED_EDGE('',*,*,#2069,.F.);
#2926=ORIENTED_EDGE('',*,*,#2070,.T.);
#2927=ORIENTED_EDGE('',*,*,#2071,.T.);
#2928=ORIENTED_EDGE('',*,*,#2072,.T.);
#2929=ORIENTED_EDGE('',*,*,#2073,.T.);
#2930=ORIENTED_EDGE('',*,*,#2050,.T.);
#2931=ORIENTED_EDGE('',*,*,#2074,.T.);
#2932=ORIENTED_EDGE('',*,*,#2054,.F.);
#2933=ORIENTED_EDGE('',*,*,#2075,.F.);
#2934=ORIENTED_EDGE('',*,*,#2076,.F.);
#2935=ORIENTED_EDGE('',*,*,#2077,.T.);
#2936=ORIENTED_EDGE('',*,*,#2078,.T.);
#2937=ORIENTED_EDGE('',*,*,#2079,.F.);
#2938=ORIENTED_EDGE('',*,*,#2080,.F.);
#2939=ORIENTED_EDGE('',*,*,#2055,.T.);
#2940=ORIENTED_EDGE('',*,*,#2074,.F.);
#2941=ORIENTED_EDGE('',*,*,#2049,.F.);
#2942=ORIENTED_EDGE('',*,*,#2081,.F.);
#2943=ORIENTED_EDGE('',*,*,#2065,.T.);
#2944=ORIENTED_EDGE('',*,*,#2082,.F.);
#2945=ORIENTED_EDGE('',*,*,#2070,.F.);
#2946=ORIENTED_EDGE('',*,*,#2053,.F.);
#2947=ORIENTED_EDGE('',*,*,#2083,.T.);
#2948=ORIENTED_EDGE('',*,*,#2072,.F.);
#2949=ORIENTED_EDGE('',*,*,#2084,.F.);
#2950=ORIENTED_EDGE('',*,*,#2063,.T.);
#2951=ORIENTED_EDGE('',*,*,#2085,.T.);
#2952=ORIENTED_EDGE('',*,*,#2046,.T.);
#2953=ORIENTED_EDGE('',*,*,#2075,.T.);
#2954=ORIENTED_EDGE('',*,*,#2082,.T.);
#2955=ORIENTED_EDGE('',*,*,#2064,.T.);
#2956=ORIENTED_EDGE('',*,*,#2084,.T.);
#2957=ORIENTED_EDGE('',*,*,#2071,.F.);
#2958=ORIENTED_EDGE('',*,*,#2076,.T.);
#2959=ORIENTED_EDGE('',*,*,#2086,.F.);
#2960=ORIENTED_EDGE('',*,*,#2087,.F.);
#2961=ORIENTED_EDGE('',*,*,#2088,.T.);
#2962=ORIENTED_EDGE('',*,*,#2079,.T.);
#2963=ORIENTED_EDGE('',*,*,#2089,.F.);
#2964=ORIENTED_EDGE('',*,*,#2090,.F.);
#2965=ORIENTED_EDGE('',*,*,#2086,.T.);
#2966=ORIENTED_EDGE('',*,*,#2078,.F.);
#2967=ORIENTED_EDGE('',*,*,#2091,.F.);
#2968=ORIENTED_EDGE('',*,*,#2092,.T.);
#2969=ORIENTED_EDGE('',*,*,#2089,.T.);
#2970=ORIENTED_EDGE('',*,*,#2077,.F.);
#2971=ORIENTED_EDGE('',*,*,#2088,.F.);
#2972=ORIENTED_EDGE('',*,*,#2093,.T.);
#2973=ORIENTED_EDGE('',*,*,#2091,.T.);
#2974=ORIENTED_EDGE('',*,*,#2087,.T.);
#2975=ORIENTED_EDGE('',*,*,#2090,.T.);
#2976=ORIENTED_EDGE('',*,*,#2092,.F.);
#2977=ORIENTED_EDGE('',*,*,#2093,.F.);
#2978=ORIENTED_EDGE('',*,*,#2056,.T.);
#2979=ORIENTED_EDGE('',*,*,#2080,.T.);
#2980=ORIENTED_EDGE('',*,*,#2069,.T.);
#2981=ORIENTED_EDGE('',*,*,#2059,.F.);
#2982=ORIENTED_EDGE('',*,*,#2052,.T.);
#2983=ORIENTED_EDGE('',*,*,#2061,.T.);
#2984=ORIENTED_EDGE('',*,*,#2068,.T.);
#2985=ORIENTED_EDGE('',*,*,#2083,.F.);
#2986=ORIENTED_EDGE('',*,*,#2081,.T.);
#2987=ORIENTED_EDGE('',*,*,#2048,.F.);
#2988=ORIENTED_EDGE('',*,*,#2043,.F.);
#2989=ORIENTED_EDGE('',*,*,#2066,.F.);
#2990=ORIENTED_EDGE('',*,*,#2045,.T.);
#2991=ORIENTED_EDGE('',*,*,#2047,.F.);
#2992=ORIENTED_EDGE('',*,*,#2085,.F.);
#2993=ORIENTED_EDGE('',*,*,#2062,.F.);
#2994=ORIENTED_EDGE('',*,*,#2058,.F.);
#2995=ORIENTED_EDGE('',*,*,#2094,.T.);
#2996=ORIENTED_EDGE('',*,*,#2073,.F.);
#2997=ORIENTED_EDGE('',*,*,#2094,.F.);
#2998=ORIENTED_EDGE('',*,*,#2067,.T.);
#2999=ORIENTED_EDGE('',*,*,#2095,.T.);
#3000=ORIENTED_EDGE('',*,*,#2051,.T.);
#3001=ORIENTED_EDGE('',*,*,#2095,.F.);
#3002=PLANE('',#3380);
#3003=PLANE('',#3381);
#3004=PLANE('',#3382);
#3005=PLANE('',#3383);
#3006=PLANE('',#3384);
#3007=PLANE('',#3389);
#3008=PLANE('',#3390);
#3009=PLANE('',#3391);
#3010=PLANE('',#3396);
#3011=PLANE('',#3397);
#3012=PLANE('',#3398);
#3013=PLANE('',#3403);
#3014=PLANE('',#3408);
#3015=PLANE('',#3411);
#3016=PLANE('',#3416);
#3017=PLANE('',#3419);
#3018=PLANE('',#3420);
#3019=PLANE('',#3421);
#3020=PLANE('',#3422);
#3021=PLANE('',#3423);
#3022=PLANE('',#3424);
#3023=PLANE('',#3425);
#3024=PLANE('',#3426);
#3025=PLANE('',#3427);
#3026=PLANE('',#3428);
#3027=PLANE('',#3429);
#3028=PLANE('',#3430);
#3029=PLANE('',#3431);
#3030=PLANE('',#3432);
#3031=PLANE('',#3433);
#3032=PLANE('',#3434);
#3033=PLANE('',#3435);
#3034=PLANE('',#3437);
#3035=PLANE('',#3438);
#3036=PLANE('',#3439);
#3037=PLANE('',#3440);
#3038=PLANE('',#3441);
#3039=PLANE('',#3442);
#3040=PLANE('',#3443);
#3041=PLANE('',#3444);
#3042=PLANE('',#3445);
#3043=PLANE('',#3446);
#3044=PLANE('',#3447);
#3045=PLANE('',#3448);
#3046=PLANE('',#3449);
#3047=PLANE('',#3456);
#3048=PLANE('',#3463);
#3049=PLANE('',#3468);
#3050=PLANE('',#3475);
#3051=PLANE('',#3478);
#3052=PLANE('',#3479);
#3053=PLANE('',#3480);
#3054=PLANE('',#3481);
#3055=PLANE('',#3482);
#3056=PLANE('',#3483);
#3057=PLANE('',#3484);
#3058=PLANE('',#3485);
#3059=PLANE('',#3486);
#3060=PLANE('',#3487);
#3061=PLANE('',#3488);
#3062=PLANE('',#3489);
#3063=PLANE('',#3490);
#3064=PLANE('',#3491);
#3065=PLANE('',#3492);
#3066=PLANE('',#3493);
#3067=PLANE('',#3494);
#3068=PLANE('',#3499);
#3069=PLANE('',#3503);
#3070=PLANE('',#3508);
#3071=PLANE('',#3512);
#3072=PLANE('',#3514);
#3073=PLANE('',#3518);
#3074=PLANE('',#3520);
#3075=PLANE('',#3525);
#3076=PLANE('',#3530);
#3077=PLANE('',#3534);
#3078=PLANE('',#3537);
#3079=PLANE('',#3540);
#3080=PLANE('',#3543);
#3081=PLANE('',#3546);
#3082=PLANE('',#3549);
#3083=PLANE('',#3555);
#3084=PLANE('',#3557);
#3085=PLANE('',#3561);
#3086=PLANE('',#3562);
#3087=PLANE('',#3563);
#3088=PLANE('',#3564);
#3089=PLANE('',#3565);
#3090=PLANE('',#3566);
#3091=PLANE('',#3567);
#3092=PLANE('',#3568);
#3093=PLANE('',#3569);
#3094=PLANE('',#3570);
#3095=PLANE('',#3571);
#3096=PLANE('',#3572);
#3097=PLANE('',#3573);
#3098=PLANE('',#3574);
#3099=PLANE('',#3576);
#3100=PLANE('',#3577);
#3101=PLANE('',#3580);
#3102=PLANE('',#3583);
#3103=PLANE('',#3586);
#3104=PLANE('',#3589);
#3105=PLANE('',#3590);
#3106=PLANE('',#3591);
#3107=PLANE('',#3596);
#3108=PLANE('',#3597);
#3109=PLANE('',#3598);
#3110=PLANE('',#3599);
#3111=PLANE('',#3600);
#3112=PLANE('',#3602);
#3113=PLANE('',#3603);
#3114=PLANE('',#3607);
#3115=PLANE('',#3611);
#3116=PLANE('',#3612);
#3117=PLANE('',#3616);
#3118=PLANE('',#3620);
#3119=PLANE('',#3621);
#3120=PLANE('',#3622);
#3121=PLANE('',#3623);
#3122=PLANE('',#3624);
#3123=PLANE('',#3625);
#3124=PLANE('',#3626);
#3125=PLANE('',#3627);
#3126=PLANE('',#3628);
#3127=ADVANCED_FACE('',(#236),#3002,.T.);
#3128=ADVANCED_FACE('',(#237),#3003,.T.);
#3129=ADVANCED_FACE('',(#238),#3004,.F.);
#3130=ADVANCED_FACE('',(#239),#3005,.F.);
#3131=ADVANCED_FACE('',(#240),#3006,.T.);
#3132=ADVANCED_FACE('',(#241),#3007,.T.);
#3133=ADVANCED_FACE('',(#242),#3008,.T.);
#3134=ADVANCED_FACE('',(#243),#3009,.T.);
#3135=ADVANCED_FACE('',(#244),#3010,.T.);
#3136=ADVANCED_FACE('',(#245),#3011,.T.);
#3137=ADVANCED_FACE('',(#246),#3012,.T.);
#3138=ADVANCED_FACE('',(#247),#113,.T.);
#3139=ADVANCED_FACE('',(#248),#114,.T.);
#3140=ADVANCED_FACE('',(#249,#80,#81),#3013,.T.);
#3141=ADVANCED_FACE('',(#250),#115,.T.);
#3142=ADVANCED_FACE('',(#251),#116,.T.);
#3143=ADVANCED_FACE('',(#252),#3014,.T.);
#3144=ADVANCED_FACE('',(#253),#3015,.T.);
#3145=ADVANCED_FACE('',(#254),#117,.F.);
#3146=ADVANCED_FACE('',(#255),#118,.F.);
#3147=ADVANCED_FACE('',(#256),#3016,.T.);
#3148=ADVANCED_FACE('',(#257),#119,.F.);
#3149=ADVANCED_FACE('',(#258),#120,.F.);
#3150=ADVANCED_FACE('',(#259,#82,#83),#3017,.T.);
#3151=ADVANCED_FACE('',(#260),#3018,.F.);
#3152=ADVANCED_FACE('',(#261),#3019,.T.);
#3153=ADVANCED_FACE('',(#262),#3020,.T.);
#3154=ADVANCED_FACE('',(#263),#3021,.T.);
#3155=ADVANCED_FACE('',(#264),#3022,.T.);
#3156=ADVANCED_FACE('',(#265),#3023,.F.);
#3157=ADVANCED_FACE('',(#266),#3024,.F.);
#3158=ADVANCED_FACE('',(#267),#3025,.T.);
#3159=ADVANCED_FACE('',(#268),#3026,.F.);
#3160=ADVANCED_FACE('',(#269),#3027,.F.);
#3161=ADVANCED_FACE('',(#270),#3028,.T.);
#3162=ADVANCED_FACE('',(#271),#3029,.F.);
#3163=ADVANCED_FACE('',(#272),#3030,.F.);
#3164=ADVANCED_FACE('',(#273),#3031,.F.);
#3165=ADVANCED_FACE('',(#274),#3032,.T.);
#3166=ADVANCED_FACE('',(#275),#3033,.T.);
#3167=ADVANCED_FACE('',(#276,#84,#85),#3034,.T.);
#3168=ADVANCED_FACE('',(#277,#86,#87),#3035,.T.);
#3169=ADVANCED_FACE('',(#278),#3036,.T.);
#3170=ADVANCED_FACE('',(#279),#3037,.T.);
#3171=ADVANCED_FACE('',(#280),#3038,.T.);
#3172=ADVANCED_FACE('',(#281),#3039,.T.);
#3173=ADVANCED_FACE('',(#282),#3040,.T.);
#3174=ADVANCED_FACE('',(#283),#3041,.F.);
#3175=ADVANCED_FACE('',(#284),#3042,.F.);
#3176=ADVANCED_FACE('',(#285),#3043,.T.);
#3177=ADVANCED_FACE('',(#286,#88,#89,#90,#91),#3044,.T.);
#3178=ADVANCED_FACE('',(#287,#92,#93,#94,#95),#3045,.T.);
#3179=ADVANCED_FACE('',(#288),#3046,.T.);
#3180=ADVANCED_FACE('',(#289),#121,.T.);
#3181=ADVANCED_FACE('',(#290),#122,.T.);
#3182=ADVANCED_FACE('',(#291),#3047,.T.);
#3183=ADVANCED_FACE('',(#292),#123,.T.);
#3184=ADVANCED_FACE('',(#293),#124,.T.);
#3185=ADVANCED_FACE('',(#294,#96),#3048,.T.);
#3186=ADVANCED_FACE('',(#295,#97),#3049,.F.);
#3187=ADVANCED_FACE('',(#296),#125,.F.);
#3188=ADVANCED_FACE('',(#297),#126,.F.);
#3189=ADVANCED_FACE('',(#298),#3050,.T.);
#3190=ADVANCED_FACE('',(#299),#127,.F.);
#3191=ADVANCED_FACE('',(#300),#128,.F.);
#3192=ADVANCED_FACE('',(#301),#3051,.T.);
#3193=ADVANCED_FACE('',(#302),#3052,.T.);
#3194=ADVANCED_FACE('',(#303),#3053,.T.);
#3195=ADVANCED_FACE('',(#304),#3054,.T.);
#3196=ADVANCED_FACE('',(#305),#3055,.T.);
#3197=ADVANCED_FACE('',(#306),#3056,.T.);
#3198=ADVANCED_FACE('',(#307),#3057,.T.);
#3199=ADVANCED_FACE('',(#308),#3058,.F.);
#3200=ADVANCED_FACE('',(#309),#3059,.F.);
#3201=ADVANCED_FACE('',(#310),#3060,.T.);
#3202=ADVANCED_FACE('',(#311),#3061,.T.);
#3203=ADVANCED_FACE('',(#312),#3062,.F.);
#3204=ADVANCED_FACE('',(#313),#3063,.F.);
#3205=ADVANCED_FACE('',(#314),#3064,.T.);
#3206=ADVANCED_FACE('',(#315),#3065,.F.);
#3207=ADVANCED_FACE('',(#316),#3066,.F.);
#3208=ADVANCED_FACE('',(#317),#3067,.T.);
#3209=ADVANCED_FACE('',(#318),#129,.F.);
#3210=ADVANCED_FACE('',(#319,#98),#3068,.F.);
#3211=ADVANCED_FACE('',(#320),#130,.T.);
#3212=ADVANCED_FACE('',(#321,#99),#3069,.T.);
#3213=ADVANCED_FACE('',(#322),#51,.F.);
#3214=ADVANCED_FACE('',(#323,#100),#3070,.F.);
#3215=ADVANCED_FACE('',(#324),#131,.T.);
#3216=ADVANCED_FACE('',(#325,#101),#3071,.T.);
#3217=ADVANCED_FACE('',(#326),#3072,.F.);
#3218=ADVANCED_FACE('',(#327),#132,.T.);
#3219=ADVANCED_FACE('',(#328),#3073,.T.);
#3220=ADVANCED_FACE('',(#329),#3074,.F.);
#3221=ADVANCED_FACE('',(#330),#3075,.F.);
#3222=ADVANCED_FACE('',(#331),#3076,.T.);
#3223=ADVANCED_FACE('',(#332),#133,.T.);
#3224=ADVANCED_FACE('',(#333),#3077,.T.);
#3225=ADVANCED_FACE('',(#334),#134,.T.);
#3226=ADVANCED_FACE('',(#335),#3078,.T.);
#3227=ADVANCED_FACE('',(#336),#135,.F.);
#3228=ADVANCED_FACE('',(#337),#3079,.T.);
#3229=ADVANCED_FACE('',(#338),#136,.F.);
#3230=ADVANCED_FACE('',(#339),#3080,.T.);
#3231=ADVANCED_FACE('',(#340),#137,.F.);
#3232=ADVANCED_FACE('',(#341),#3081,.T.);
#3233=ADVANCED_FACE('',(#342),#138,.F.);
#3234=ADVANCED_FACE('',(#343,#102),#3082,.T.);
#3235=ADVANCED_FACE('',(#344),#139,.T.);
#3236=ADVANCED_FACE('',(#345),#3083,.T.);
#3237=ADVANCED_FACE('',(#346),#140,.T.);
#3238=ADVANCED_FACE('',(#347),#3084,.T.);
#3239=ADVANCED_FACE('',(#348),#141,.T.);
#3240=ADVANCED_FACE('',(#349),#142,.T.);
#3241=ADVANCED_FACE('',(#350),#3085,.F.);
#3242=ADVANCED_FACE('',(#351),#3086,.F.);
#3243=ADVANCED_FACE('',(#352),#3087,.T.);
#3244=ADVANCED_FACE('',(#353),#3088,.F.);
#3245=ADVANCED_FACE('',(#354),#3089,.T.);
#3246=ADVANCED_FACE('',(#355),#3090,.T.);
#3247=ADVANCED_FACE('',(#356),#3091,.F.);
#3248=ADVANCED_FACE('',(#357),#3092,.T.);
#3249=ADVANCED_FACE('',(#358),#3093,.F.);
#3250=ADVANCED_FACE('',(#359),#3094,.T.);
#3251=ADVANCED_FACE('',(#360),#3095,.F.);
#3252=ADVANCED_FACE('',(#361),#3096,.F.);
#3253=ADVANCED_FACE('',(#362),#3097,.T.);
#3254=ADVANCED_FACE('',(#363),#3098,.F.);
#3255=ADVANCED_FACE('',(#364,#103),#3099,.F.);
#3256=ADVANCED_FACE('',(#365,#104),#3100,.T.);
#3257=ADVANCED_FACE('',(#366,#105),#3101,.F.);
#3258=ADVANCED_FACE('',(#367,#106),#3102,.T.);
#3259=ADVANCED_FACE('',(#368,#107),#3103,.F.);
#3260=ADVANCED_FACE('',(#369),#3104,.T.);
#3261=ADVANCED_FACE('',(#370),#3105,.F.);
#3262=ADVANCED_FACE('',(#371),#3106,.T.);
#3263=ADVANCED_FACE('',(#372),#143,.F.);
#3264=ADVANCED_FACE('',(#373),#144,.F.);
#3265=ADVANCED_FACE('',(#374),#145,.T.);
#3266=ADVANCED_FACE('',(#375),#146,.T.);
#3267=ADVANCED_FACE('',(#376),#3107,.F.);
#3268=ADVANCED_FACE('',(#377),#3108,.T.);
#3269=ADVANCED_FACE('',(#378),#3109,.T.);
#3270=ADVANCED_FACE('',(#379),#3110,.F.);
#3271=ADVANCED_FACE('',(#380),#3111,.F.);
#3272=ADVANCED_FACE('',(#381),#3112,.T.);
#3273=ADVANCED_FACE('',(#382,#108),#3113,.T.);
#3274=ADVANCED_FACE('',(#383,#109),#3114,.F.);
#3275=ADVANCED_FACE('',(#384),#3115,.T.);
#3276=ADVANCED_FACE('',(#385,#110),#3116,.T.);
#3277=ADVANCED_FACE('',(#386,#111),#3117,.F.);
#3278=ADVANCED_FACE('',(#387,#112),#3118,.F.);
#3279=ADVANCED_FACE('',(#388),#3119,.T.);
#3280=ADVANCED_FACE('',(#389),#3120,.F.);
#3281=ADVANCED_FACE('',(#390),#3121,.F.);
#3282=ADVANCED_FACE('',(#391),#3122,.F.);
#3283=ADVANCED_FACE('',(#392),#3123,.F.);
#3284=ADVANCED_FACE('',(#393),#3124,.T.);
#3285=ADVANCED_FACE('',(#394),#3125,.T.);
#3286=ADVANCED_FACE('',(#395),#3126,.T.);
#3287=ADVANCED_FACE('',(#396),#147,.T.);
#3288=ADVANCED_FACE('',(#397),#148,.T.);
#3289=ADVANCED_FACE('',(#398),#149,.T.);
#3290=ADVANCED_FACE('',(#399),#150,.T.);
#3291=ADVANCED_FACE('',(#400),#151,.F.);
#3292=ADVANCED_FACE('',(#401),#152,.F.);
#3293=CLOSED_SHELL('',(#3127,#3128,#3129,#3130,#3131,#3132,#3133,#3134,
#3135,#3136,#3137,#3138,#3139,#3140,#3141,#3142,#3143,#3144,#3145,#3146,
#3147,#3148,#3149,#3150,#3151,#3152,#3153,#3154,#3155,#3156,#3157,#3158,
#3159,#3160,#3161,#3162,#3163,#3164,#3165,#3166));
#3294=CLOSED_SHELL('',(#3167,#3168,#3169,#3170,#3171,#3172,#3173,#3174,
#3175,#3176,#3177,#3178,#3179,#3180,#3181,#3182,#3183,#3184,#3185,#3186,
#3187,#3188,#3189,#3190,#3191,#3192,#3193,#3194,#3195,#3196,#3197,#3198,
#3199,#3200,#3201,#3202,#3203,#3204,#3205,#3206,#3207,#3208));
#3295=CLOSED_SHELL('',(#3209,#3210,#3211,#3212,#3213,#3214,#3215,#3216));
#3296=CLOSED_SHELL('',(#3217,#3218,#3219));
#3297=CLOSED_SHELL('',(#3220,#3221,#3222,#3223,#3224,#3225,#3226,#3227,
#3228,#3229,#3230,#3231,#3232,#3233,#3234,#3235,#3236,#3237,#3238,#3239,
#3240,#3241,#3242,#3243,#3244,#3245,#3246,#3247,#3248,#3249,#3250,#3251,
#3252,#3253,#3254));
#3298=CLOSED_SHELL('',(#3255,#3256,#3257,#3258,#3259,#3260,#3261,#3262,
#3263,#3264,#3265,#3266,#3267,#3268,#3269,#3270,#3271));
#3299=CLOSED_SHELL('',(#3272,#3273,#3274,#3275,#3276,#3277,#3278,#3279,
#3280,#3281,#3282,#3283,#3284,#3285,#3286,#3287,#3288,#3289,#3290,#3291,
#3292));
#3300=DERIVED_UNIT_ELEMENT(#3314,1.);
#3301=DERIVED_UNIT_ELEMENT(#5507,-3.);
#3302=DERIVED_UNIT_ELEMENT(#3314,1.);
#3303=DERIVED_UNIT_ELEMENT(#5507,-3.);
#3304=DERIVED_UNIT_ELEMENT(#3314,1.);
#3305=DERIVED_UNIT_ELEMENT(#5507,-3.);
#3306=DERIVED_UNIT_ELEMENT(#3314,1.);
#3307=DERIVED_UNIT_ELEMENT(#5507,-3.);
#3308=DERIVED_UNIT_ELEMENT(#3314,1.);
#3309=DERIVED_UNIT_ELEMENT(#5507,-3.);
#3310=DERIVED_UNIT_ELEMENT(#3314,1.);
#3311=DERIVED_UNIT_ELEMENT(#5507,-3.);
#3312=DERIVED_UNIT_ELEMENT(#3314,1.);
#3313=DERIVED_UNIT_ELEMENT(#5507,-3.);
#3314=(
MASS_UNIT()
NAMED_UNIT(*)
SI_UNIT(.KILO.,.GRAM.)
);
#3315=DERIVED_UNIT((#3300,#3301));
#3316=DERIVED_UNIT((#3302,#3303));
#3317=DERIVED_UNIT((#3304,#3305));
#3318=DERIVED_UNIT((#3306,#3307));
#3319=DERIVED_UNIT((#3308,#3309));
#3320=DERIVED_UNIT((#3310,#3311));
#3321=DERIVED_UNIT((#3312,#3313));
#3322=MEASURE_REPRESENTATION_ITEM('density measure',
POSITIVE_RATIO_MEASURE(7850.),#3315);
#3323=MEASURE_REPRESENTATION_ITEM('density measure',
POSITIVE_RATIO_MEASURE(7850.),#3316);
#3324=MEASURE_REPRESENTATION_ITEM('density measure',
POSITIVE_RATIO_MEASURE(7850.),#3317);
#3325=MEASURE_REPRESENTATION_ITEM('density measure',
POSITIVE_RATIO_MEASURE(7850.),#3318);
#3326=MEASURE_REPRESENTATION_ITEM('density measure',
POSITIVE_RATIO_MEASURE(7850.),#3319);
#3327=MEASURE_REPRESENTATION_ITEM('density measure',
POSITIVE_RATIO_MEASURE(7850.),#3320);
#3328=MEASURE_REPRESENTATION_ITEM('density measure',
POSITIVE_RATIO_MEASURE(7850.),#3321);
#3329=PROPERTY_DEFINITION_REPRESENTATION(#3364,#3343);
#3330=PROPERTY_DEFINITION_REPRESENTATION(#3365,#3344);
#3331=PROPERTY_DEFINITION_REPRESENTATION(#3366,#3345);
#3332=PROPERTY_DEFINITION_REPRESENTATION(#3367,#3346);
#3333=PROPERTY_DEFINITION_REPRESENTATION(#3368,#3347);
#3334=PROPERTY_DEFINITION_REPRESENTATION(#3369,#3348);
#3335=PROPERTY_DEFINITION_REPRESENTATION(#3370,#3349);
#3336=PROPERTY_DEFINITION_REPRESENTATION(#3371,#3350);
#3337=PROPERTY_DEFINITION_REPRESENTATION(#3372,#3351);
#3338=PROPERTY_DEFINITION_REPRESENTATION(#3373,#3352);
#3339=PROPERTY_DEFINITION_REPRESENTATION(#3374,#3353);
#3340=PROPERTY_DEFINITION_REPRESENTATION(#3375,#3354);
#3341=PROPERTY_DEFINITION_REPRESENTATION(#3376,#3355);
#3342=PROPERTY_DEFINITION_REPRESENTATION(#3377,#3356);
#3343=REPRESENTATION('material name',(#3357),#5498);
#3344=REPRESENTATION('density',(#3322),#5498);
#3345=REPRESENTATION('material name',(#3358),#5499);
#3346=REPRESENTATION('density',(#3323),#5499);
#3347=REPRESENTATION('material name',(#3359),#5500);
#3348=REPRESENTATION('density',(#3324),#5500);
#3349=REPRESENTATION('material name',(#3360),#5501);
#3350=REPRESENTATION('density',(#3325),#5501);
#3351=REPRESENTATION('material name',(#3361),#5502);
#3352=REPRESENTATION('density',(#3326),#5502);
#3353=REPRESENTATION('material name',(#3362),#5503);
#3354=REPRESENTATION('density',(#3327),#5503);
#3355=REPRESENTATION('material name',(#3363),#5504);
#3356=REPRESENTATION('density',(#3328),#5504);
#3357=DESCRIPTIVE_REPRESENTATION_ITEM('Steel','Steel');
#3358=DESCRIPTIVE_REPRESENTATION_ITEM('Steel','Steel');
#3359=DESCRIPTIVE_REPRESENTATION_ITEM('Steel','Steel');
#3360=DESCRIPTIVE_REPRESENTATION_ITEM('Steel','Steel');
#3361=DESCRIPTIVE_REPRESENTATION_ITEM('Steel','Steel');
#3362=DESCRIPTIVE_REPRESENTATION_ITEM('Steel','Steel');
#3363=DESCRIPTIVE_REPRESENTATION_ITEM('Steel','Steel');
#3364=PROPERTY_DEFINITION('material property','material name',#5546);
#3365=PROPERTY_DEFINITION('material property','density of part',#5546);
#3366=PROPERTY_DEFINITION('material property','material name',#5547);
#3367=PROPERTY_DEFINITION('material property','density of part',#5547);
#3368=PROPERTY_DEFINITION('material property','material name',#5548);
#3369=PROPERTY_DEFINITION('material property','density of part',#5548);
#3370=PROPERTY_DEFINITION('material property','material name',#5549);
#3371=PROPERTY_DEFINITION('material property','density of part',#5549);
#3372=PROPERTY_DEFINITION('material property','material name',#5550);
#3373=PROPERTY_DEFINITION('material property','density of part',#5550);
#3374=PROPERTY_DEFINITION('material property','material name',#5551);
#3375=PROPERTY_DEFINITION('material property','density of part',#5551);
#3376=PROPERTY_DEFINITION('material property','material name',#5552);
#3377=PROPERTY_DEFINITION('material property','density of part',#5552);
#3378=AXIS2_PLACEMENT_3D('',#4549,#3645,#3646);
#3379=AXIS2_PLACEMENT_3D('',#4550,#3647,#3648);
#3380=AXIS2_PLACEMENT_3D('',#4551,#3649,#3650);
#3381=AXIS2_PLACEMENT_3D('',#4560,#3655,#3656);
#3382=AXIS2_PLACEMENT_3D('',#4566,#3660,#3661);
#3383=AXIS2_PLACEMENT_3D('',#4572,#3665,#3666);
#3384=AXIS2_PLACEMENT_3D('',#4575,#3669,#3670);
#3385=AXIS2_PLACEMENT_3D('',#4584,#3674,#3675);
#3386=AXIS2_PLACEMENT_3D('',#4588,#3677,#3678);
#3387=AXIS2_PLACEMENT_3D('',#4596,#3682,#3683);
#3388=AXIS2_PLACEMENT_3D('',#4599,#3685,#3686);
#3389=AXIS2_PLACEMENT_3D('',#4600,#3687,#3688);
#3390=AXIS2_PLACEMENT_3D('',#4622,#3700,#3701);
#3391=AXIS2_PLACEMENT_3D('',#4644,#3713,#3714);
#3392=AXIS2_PLACEMENT_3D('',#4650,#3717,#3718);
#3393=AXIS2_PLACEMENT_3D('',#4654,#3720,#3721);
#3394=AXIS2_PLACEMENT_3D('',#4659,#3724,#3725);
#3395=AXIS2_PLACEMENT_3D('',#4662,#3727,#3728);
#3396=AXIS2_PLACEMENT_3D('',#4663,#3729,#3730);
#3397=AXIS2_PLACEMENT_3D('',#4682,#3741,#3742);
#3398=AXIS2_PLACEMENT_3D('',#4701,#3753,#3754);
#3399=AXIS2_PLACEMENT_3D('',#4707,#3758,#3759);
#3400=AXIS2_PLACEMENT_3D('',#4708,#3760,#3761);
#3401=AXIS2_PLACEMENT_3D('',#4709,#3762,#3763);
#3402=AXIS2_PLACEMENT_3D('',#4712,#3765,#3766);
#3403=AXIS2_PLACEMENT_3D('',#4713,#3767,#3768);
#3404=AXIS2_PLACEMENT_3D('',#4725,#3775,#3776);
#3405=AXIS2_PLACEMENT_3D('',#4726,#3777,#3778);
#3406=AXIS2_PLACEMENT_3D('',#4727,#3779,#3780);
#3407=AXIS2_PLACEMENT_3D('',#4728,#3781,#3782);
#3408=AXIS2_PLACEMENT_3D('',#4729,#3783,#3784);
#3409=AXIS2_PLACEMENT_3D('',#4733,#3787,#3788);
#3410=AXIS2_PLACEMENT_3D('',#4736,#3790,#3791);
#3411=AXIS2_PLACEMENT_3D('',#4737,#3792,#3793);
#3412=AXIS2_PLACEMENT_3D('',#4740,#3795,#3796);
#3413=AXIS2_PLACEMENT_3D('',#4743,#3798,#3799);
#3414=AXIS2_PLACEMENT_3D('',#4745,#3801,#3802);
#3415=AXIS2_PLACEMENT_3D('',#4747,#3804,#3805);
#3416=AXIS2_PLACEMENT_3D('',#4749,#3807,#3808);
#3417=AXIS2_PLACEMENT_3D('',#4751,#3810,#3811);
#3418=AXIS2_PLACEMENT_3D('',#4752,#3812,#3813);
#3419=AXIS2_PLACEMENT_3D('',#4754,#3815,#3816);
#3420=AXIS2_PLACEMENT_3D('',#4763,#3821,#3822);
#3421=AXIS2_PLACEMENT_3D('',#4765,#3824,#3825);
#3422=AXIS2_PLACEMENT_3D('',#4767,#3827,#3828);
#3423=AXIS2_PLACEMENT_3D('',#4768,#3829,#3830);
#3424=AXIS2_PLACEMENT_3D('',#4770,#3832,#3833);
#3425=AXIS2_PLACEMENT_3D('',#4772,#3835,#3836);
#3426=AXIS2_PLACEMENT_3D('',#4773,#3837,#3838);
#3427=AXIS2_PLACEMENT_3D('',#4775,#3840,#3841);
#3428=AXIS2_PLACEMENT_3D('',#4777,#3843,#3844);
#3429=AXIS2_PLACEMENT_3D('',#4778,#3845,#3846);
#3430=AXIS2_PLACEMENT_3D('',#4780,#3848,#3849);
#3431=AXIS2_PLACEMENT_3D('',#4782,#3851,#3852);
#3432=AXIS2_PLACEMENT_3D('',#4783,#3853,#3854);
#3433=AXIS2_PLACEMENT_3D('',#4786,#3857,#3858);
#3434=AXIS2_PLACEMENT_3D('',#4788,#3860,#3861);
#3435=AXIS2_PLACEMENT_3D('',#4790,#3863,#3864);
#3436=AXIS2_PLACEMENT_3D('',#4791,#3865,#3866);
#3437=AXIS2_PLACEMENT_3D('',#4792,#3867,#3868);
#3438=AXIS2_PLACEMENT_3D('',#4817,#3881,#3882);
#3439=AXIS2_PLACEMENT_3D('',#4842,#3895,#3896);
#3440=AXIS2_PLACEMENT_3D('',#4851,#3901,#3902);
#3441=AXIS2_PLACEMENT_3D('',#4857,#3906,#3907);
#3442=AXIS2_PLACEMENT_3D('',#4863,#3911,#3912);
#3443=AXIS2_PLACEMENT_3D('',#4866,#3915,#3916);
#3444=AXIS2_PLACEMENT_3D('',#4875,#3921,#3922);
#3445=AXIS2_PLACEMENT_3D('',#4881,#3926,#3927);
#3446=AXIS2_PLACEMENT_3D('',#4887,#3931,#3932);
#3447=AXIS2_PLACEMENT_3D('',#4890,#3935,#3936);
#3448=AXIS2_PLACEMENT_3D('',#4915,#3949,#3950);
#3449=AXIS2_PLACEMENT_3D('',#4940,#3963,#3964);
#3450=AXIS2_PLACEMENT_3D('',#4949,#3969,#3970);
#3451=AXIS2_PLACEMENT_3D('',#4950,#3971,#3972);
#3452=AXIS2_PLACEMENT_3D('',#4951,#3973,#3974);
#3453=AXIS2_PLACEMENT_3D('',#4952,#3975,#3976);
#3454=AXIS2_PLACEMENT_3D('',#4954,#3977,#3978);
#3455=AXIS2_PLACEMENT_3D('',#4957,#3980,#3981);
#3456=AXIS2_PLACEMENT_3D('',#4958,#3982,#3983);
#3457=AXIS2_PLACEMENT_3D('',#4964,#3987,#3988);
#3458=AXIS2_PLACEMENT_3D('',#4965,#3989,#3990);
#3459=AXIS2_PLACEMENT_3D('',#4966,#3991,#3992);
#3460=AXIS2_PLACEMENT_3D('',#4967,#3993,#3994);
#3461=AXIS2_PLACEMENT_3D('',#4968,#3995,#3996);
#3462=AXIS2_PLACEMENT_3D('',#4969,#3997,#3998);
#3463=AXIS2_PLACEMENT_3D('',#4970,#3999,#4000);
#3464=AXIS2_PLACEMENT_3D('',#4972,#4001,#4002);
#3465=AXIS2_PLACEMENT_3D('',#4974,#4003,#4004);
#3466=AXIS2_PLACEMENT_3D('',#4977,#4006,#4007);
#3467=AXIS2_PLACEMENT_3D('',#4979,#4008,#4009);
#3468=AXIS2_PLACEMENT_3D('',#4981,#4011,#4012);
#3469=AXIS2_PLACEMENT_3D('',#4983,#4013,#4014);
#3470=AXIS2_PLACEMENT_3D('',#4986,#4016,#4017);
#3471=AXIS2_PLACEMENT_3D('',#4988,#4018,#4019);
#3472=AXIS2_PLACEMENT_3D('',#4991,#4021,#4022);
#3473=AXIS2_PLACEMENT_3D('',#4992,#4023,#4024);
#3474=AXIS2_PLACEMENT_3D('',#4994,#4026,#4027);
#3475=AXIS2_PLACEMENT_3D('',#4996,#4029,#4030);
#3476=AXIS2_PLACEMENT_3D('',#4998,#4032,#4033);
#3477=AXIS2_PLACEMENT_3D('',#4999,#4034,#4035);
#3478=AXIS2_PLACEMENT_3D('',#5001,#4037,#4038);
#3479=AXIS2_PLACEMENT_3D('',#5002,#4039,#4040);
#3480=AXIS2_PLACEMENT_3D('',#5005,#4043,#4044);
#3481=AXIS2_PLACEMENT_3D('',#5007,#4046,#4047);
#3482=AXIS2_PLACEMENT_3D('',#5009,#4049,#4050);
#3483=AXIS2_PLACEMENT_3D('',#5010,#4051,#4052);
#3484=AXIS2_PLACEMENT_3D('',#5013,#4055,#4056);
#3485=AXIS2_PLACEMENT_3D('',#5015,#4058,#4059);
#3486=AXIS2_PLACEMENT_3D('',#5017,#4061,#4062);
#3487=AXIS2_PLACEMENT_3D('',#5018,#4063,#4064);
#3488=AXIS2_PLACEMENT_3D('',#5021,#4067,#4068);
#3489=AXIS2_PLACEMENT_3D('',#5023,#4070,#4071);
#3490=AXIS2_PLACEMENT_3D('',#5025,#4073,#4074);
#3491=AXIS2_PLACEMENT_3D('',#5026,#4075,#4076);
#3492=AXIS2_PLACEMENT_3D('',#5029,#4079,#4080);
#3493=AXIS2_PLACEMENT_3D('',#5031,#4082,#4083);
#3494=AXIS2_PLACEMENT_3D('',#5033,#4085,#4086);
#3495=AXIS2_PLACEMENT_3D('',#5034,#4087,#4088);
#3496=AXIS2_PLACEMENT_3D('',#5035,#4089,#4090);
#3497=AXIS2_PLACEMENT_3D('',#5037,#4091,#4092);
#3498=AXIS2_PLACEMENT_3D('',#5040,#4094,#4095);
#3499=AXIS2_PLACEMENT_3D('',#5041,#4096,#4097);
#3500=AXIS2_PLACEMENT_3D('',#5043,#4098,#4099);
#3501=AXIS2_PLACEMENT_3D('',#5044,#4100,#4101);
#3502=AXIS2_PLACEMENT_3D('',#5047,#4103,#4104);
#3503=AXIS2_PLACEMENT_3D('',#5048,#4105,#4106);
#3504=AXIS2_PLACEMENT_3D('',#5050,#4107,#4108);
#3505=AXIS2_PLACEMENT_3D('',#5051,#4109,#4110);
#3506=AXIS2_PLACEMENT_3D('',#5053,#4111,#4112);
#3507=AXIS2_PLACEMENT_3D('',#5054,#4113,#4114);
#3508=AXIS2_PLACEMENT_3D('',#5055,#4115,#4116);
#3509=AXIS2_PLACEMENT_3D('',#5057,#4117,#4118);
#3510=AXIS2_PLACEMENT_3D('',#5058,#4119,#4120);
#3511=AXIS2_PLACEMENT_3D('',#5061,#4122,#4123);
#3512=AXIS2_PLACEMENT_3D('',#5062,#4124,#4125);
#3513=AXIS2_PLACEMENT_3D('',#5063,#4126,#4127);
#3514=AXIS2_PLACEMENT_3D('',#5064,#4128,#4129);
#3515=AXIS2_PLACEMENT_3D('',#5066,#4130,#4131);
#3516=AXIS2_PLACEMENT_3D('',#5067,#4132,#4133);
#3517=AXIS2_PLACEMENT_3D('',#5069,#4134,#4135);
#3518=AXIS2_PLACEMENT_3D('',#5071,#4137,#4138);
#3519=AXIS2_PLACEMENT_3D('',#5072,#4139,#4140);
#3520=AXIS2_PLACEMENT_3D('',#5073,#4141,#4142);
#3521=AXIS2_PLACEMENT_3D('',#5080,#4145,#4146);
#3522=AXIS2_PLACEMENT_3D('',#5084,#4148,#4149);
#3523=AXIS2_PLACEMENT_3D('',#5092,#4153,#4154);
#3524=AXIS2_PLACEMENT_3D('',#5096,#4156,#4157);
#3525=AXIS2_PLACEMENT_3D('',#5098,#4159,#4160);
#3526=AXIS2_PLACEMENT_3D('',#5103,#4162,#4163);
#3527=AXIS2_PLACEMENT_3D('',#5107,#4165,#4166);
#3528=AXIS2_PLACEMENT_3D('',#5115,#4170,#4171);
#3529=AXIS2_PLACEMENT_3D('',#5119,#4173,#4174);
#3530=AXIS2_PLACEMENT_3D('',#5123,#4177,#4178);
#3531=AXIS2_PLACEMENT_3D('',#5137,#4186,#4187);
#3532=AXIS2_PLACEMENT_3D('',#5139,#4188,#4189);
#3533=AXIS2_PLACEMENT_3D('',#5142,#4191,#4192);
#3534=AXIS2_PLACEMENT_3D('',#5143,#4193,#4194);
#3535=AXIS2_PLACEMENT_3D('',#5167,#4208,#4209);
#3536=AXIS2_PLACEMENT_3D('',#5170,#4211,#4212);
#3537=AXIS2_PLACEMENT_3D('',#5171,#4213,#4214);
#3538=AXIS2_PLACEMENT_3D('',#5182,#4221,#4222);
#3539=AXIS2_PLACEMENT_3D('',#5185,#4224,#4225);
#3540=AXIS2_PLACEMENT_3D('',#5186,#4226,#4227);
#3541=AXIS2_PLACEMENT_3D('',#5190,#4230,#4231);
#3542=AXIS2_PLACEMENT_3D('',#5193,#4233,#4234);
#3543=AXIS2_PLACEMENT_3D('',#5194,#4235,#4236);
#3544=AXIS2_PLACEMENT_3D('',#5203,#4242,#4243);
#3545=AXIS2_PLACEMENT_3D('',#5206,#4245,#4246);
#3546=AXIS2_PLACEMENT_3D('',#5207,#4247,#4248);
#3547=AXIS2_PLACEMENT_3D('',#5211,#4251,#4252);
#3548=AXIS2_PLACEMENT_3D('',#5212,#4253,#4254);
#3549=AXIS2_PLACEMENT_3D('',#5213,#4255,#4256);
#3550=AXIS2_PLACEMENT_3D('',#5217,#4258,#4259);
#3551=AXIS2_PLACEMENT_3D('',#5219,#4260,#4261);
#3552=AXIS2_PLACEMENT_3D('',#5222,#4263,#4264);
#3553=AXIS2_PLACEMENT_3D('',#5223,#4265,#4266);
#3554=AXIS2_PLACEMENT_3D('',#5225,#4267,#4268);
#3555=AXIS2_PLACEMENT_3D('',#5227,#4270,#4271);
#3556=AXIS2_PLACEMENT_3D('',#5234,#4276,#4277);
#3557=AXIS2_PLACEMENT_3D('',#5236,#4279,#4280);
#3558=AXIS2_PLACEMENT_3D('',#5243,#4285,#4286);
#3559=AXIS2_PLACEMENT_3D('',#5244,#4287,#4288);
#3560=AXIS2_PLACEMENT_3D('',#5245,#4289,#4290);
#3561=AXIS2_PLACEMENT_3D('',#5246,#4291,#4292);
#3562=AXIS2_PLACEMENT_3D('',#5250,#4295,#4296);
#3563=AXIS2_PLACEMENT_3D('',#5254,#4299,#4300);
#3564=AXIS2_PLACEMENT_3D('',#5256,#4302,#4303);
#3565=AXIS2_PLACEMENT_3D('',#5257,#4304,#4305);
#3566=AXIS2_PLACEMENT_3D('',#5261,#4308,#4309);
#3567=AXIS2_PLACEMENT_3D('',#5265,#4312,#4313);
#3568=AXIS2_PLACEMENT_3D('',#5267,#4315,#4316);
#3569=AXIS2_PLACEMENT_3D('',#5268,#4317,#4318);
#3570=AXIS2_PLACEMENT_3D('',#5270,#4320,#4321);
#3571=AXIS2_PLACEMENT_3D('',#5272,#4323,#4324);
#3572=AXIS2_PLACEMENT_3D('',#5273,#4325,#4326);
#3573=AXIS2_PLACEMENT_3D('',#5275,#4328,#4329);
#3574=AXIS2_PLACEMENT_3D('',#5277,#4331,#4332);
#3575=AXIS2_PLACEMENT_3D('',#5278,#4333,#4334);
#3576=AXIS2_PLACEMENT_3D('',#5279,#4335,#4336);
#3577=AXIS2_PLACEMENT_3D('',#5296,#4345,#4346);
#3578=AXIS2_PLACEMENT_3D('',#5300,#4348,#4349);
#3579=AXIS2_PLACEMENT_3D('',#5303,#4351,#4352);
#3580=AXIS2_PLACEMENT_3D('',#5304,#4353,#4354);
#3581=AXIS2_PLACEMENT_3D('',#5307,#4355,#4356);
#3582=AXIS2_PLACEMENT_3D('',#5311,#4359,#4360);
#3583=AXIS2_PLACEMENT_3D('',#5312,#4361,#4362);
#3584=AXIS2_PLACEMENT_3D('',#5317,#4364,#4365);
#3585=AXIS2_PLACEMENT_3D('',#5322,#4368,#4369);
#3586=AXIS2_PLACEMENT_3D('',#5323,#4370,#4371);
#3587=AXIS2_PLACEMENT_3D('',#5328,#4373,#4374);
#3588=AXIS2_PLACEMENT_3D('',#5333,#4377,#4378);
#3589=AXIS2_PLACEMENT_3D('',#5334,#4379,#4380);
#3590=AXIS2_PLACEMENT_3D('',#5338,#4384,#4385);
#3591=AXIS2_PLACEMENT_3D('',#5342,#4389,#4390);
#3592=AXIS2_PLACEMENT_3D('',#5343,#4391,#4392);
#3593=AXIS2_PLACEMENT_3D('',#5345,#4394,#4395);
#3594=AXIS2_PLACEMENT_3D('',#5347,#4397,#4398);
#3595=AXIS2_PLACEMENT_3D('',#5348,#4399,#4400);
#3596=AXIS2_PLACEMENT_3D('',#5349,#4401,#4402);
#3597=AXIS2_PLACEMENT_3D('',#5355,#4406,#4407);
#3598=AXIS2_PLACEMENT_3D('',#5359,#4410,#4411);
#3599=AXIS2_PLACEMENT_3D('',#5363,#4414,#4415);
#3600=AXIS2_PLACEMENT_3D('',#5365,#4417,#4418);
#3601=AXIS2_PLACEMENT_3D('',#5366,#4419,#4420);
#3602=AXIS2_PLACEMENT_3D('',#5367,#4421,#4422);
#3603=AXIS2_PLACEMENT_3D('',#5376,#4427,#4428);
#3604=AXIS2_PLACEMENT_3D('',#5380,#4430,#4431);
#3605=AXIS2_PLACEMENT_3D('',#5382,#4432,#4433);
#3606=AXIS2_PLACEMENT_3D('',#5387,#4436,#4437);
#3607=AXIS2_PLACEMENT_3D('',#5388,#4438,#4439);
#3608=AXIS2_PLACEMENT_3D('',#5391,#4440,#4441);
#3609=AXIS2_PLACEMENT_3D('',#5399,#4445,#4446);
#3610=AXIS2_PLACEMENT_3D('',#5402,#4448,#4449);
#3611=AXIS2_PLACEMENT_3D('',#5403,#4450,#4451);
#3612=AXIS2_PLACEMENT_3D('',#5409,#4455,#4456);
#3613=AXIS2_PLACEMENT_3D('',#5411,#4457,#4458);
#3614=AXIS2_PLACEMENT_3D('',#5418,#4462,#4463);
#3615=AXIS2_PLACEMENT_3D('',#5420,#4464,#4465);
#3616=AXIS2_PLACEMENT_3D('',#5421,#4466,#4467);
#3617=AXIS2_PLACEMENT_3D('',#5423,#4468,#4469);
#3618=AXIS2_PLACEMENT_3D('',#5425,#4470,#4471);
#3619=AXIS2_PLACEMENT_3D('',#5432,#4475,#4476);
#3620=AXIS2_PLACEMENT_3D('',#5433,#4477,#4478);
#3621=AXIS2_PLACEMENT_3D('',#5444,#4485,#4486);
#3622=AXIS2_PLACEMENT_3D('',#5448,#4490,#4491);
#3623=AXIS2_PLACEMENT_3D('',#5452,#4495,#4496);
#3624=AXIS2_PLACEMENT_3D('',#5453,#4497,#4498);
#3625=AXIS2_PLACEMENT_3D('',#5459,#4502,#4503);
#3626=AXIS2_PLACEMENT_3D('',#5463,#4506,#4507);
#3627=AXIS2_PLACEMENT_3D('',#5467,#4510,#4511);
#3628=AXIS2_PLACEMENT_3D('',#5469,#4513,#4514);
#3629=AXIS2_PLACEMENT_3D('',#5470,#4515,#4516);
#3630=AXIS2_PLACEMENT_3D('',#5471,#4517,#4518);
#3631=AXIS2_PLACEMENT_3D('',#5472,#4519,#4520);
#3632=AXIS2_PLACEMENT_3D('',#5473,#4521,#4522);
#3633=AXIS2_PLACEMENT_3D('',#5474,#4523,#4524);
#3634=AXIS2_PLACEMENT_3D('',#5476,#4526,#4527);
#3635=AXIS2_PLACEMENT_3D('',#5478,#4529,#4530);
#3636=AXIS2_PLACEMENT_3D('',#5479,#4531,#4532);
#3637=AXIS2_PLACEMENT_3D('',#5480,#4533,#4534);
#3638=AXIS2_PLACEMENT_3D('',#5481,#4535,#4536);
#3639=AXIS2_PLACEMENT_3D('',#5482,#4537,#4538);
#3640=AXIS2_PLACEMENT_3D('',#5483,#4539,#4540);
#3641=AXIS2_PLACEMENT_3D('',#5484,#4541,#4542);
#3642=AXIS2_PLACEMENT_3D('',#5485,#4543,#4544);
#3643=AXIS2_PLACEMENT_3D('',#5486,#4545,#4546);
#3644=AXIS2_PLACEMENT_3D('',#5487,#4547,#4548);
#3645=DIRECTION('axis',(0.,0.,1.));
#3646=DIRECTION('refdir',(1.,0.,0.));
#3647=DIRECTION('axis',(0.,0.,1.));
#3648=DIRECTION('refdir',(1.,0.,0.));
#3649=DIRECTION('center_axis',(0.,-1.,-5.78241158658936E-16));
#3650=DIRECTION('ref_axis',(0.,5.78241158658936E-16,-1.));
#3651=DIRECTION('',(-3.06161699786839E-16,-5.78241158658936E-16,1.));
#3652=DIRECTION('',(1.,-1.77035296021731E-31,3.06161699786839E-16));
#3653=DIRECTION('',(-3.06161699786839E-16,-5.78241158658936E-16,1.));
#3654=DIRECTION('',(-1.,1.77035296021731E-31,-3.06161699786839E-16));
#3655=DIRECTION('center_axis',(-1.,-2.73691106313441E-47,-3.06161699786839E-16));
#3656=DIRECTION('ref_axis',(3.06161699786839E-16,0.,-1.));
#3657=DIRECTION('',(1.4960729241273E-31,-1.,-4.88654500275157E-16));
#3658=DIRECTION('',(-3.06161699786839E-16,-5.78241158658936E-16,1.));
#3659=DIRECTION('',(-1.77035296021731E-31,1.,5.78241158658936E-16));
#3660=DIRECTION('center_axis',(0.,-1.,-5.78241158658936E-16));
#3661=DIRECTION('ref_axis',(0.,5.78241158658936E-16,-1.));
#3662=DIRECTION('',(1.,-1.77035296021731E-31,3.06161699786839E-16));
#3663=DIRECTION('',(-3.06161699786839E-16,-5.78241158658936E-16,1.));
#3664=DIRECTION('',(-1.,1.77035296021731E-31,-3.06161699786839E-16));
#3665=DIRECTION('center_axis',(-1.,-2.73691106313441E-47,-3.06161699786839E-16));
#3666=DIRECTION('ref_axis',(3.06161699786839E-16,0.,-1.));
#3667=DIRECTION('',(1.4960729241273E-31,-1.,-4.88654500275157E-16));
#3668=DIRECTION('',(-1.77035296021731E-31,1.,5.78241158658936E-16));
#3669=DIRECTION('center_axis',(1.,0.,0.));
#3670=DIRECTION('ref_axis',(0.,1.,0.));
#3671=DIRECTION('',(0.,5.78241158658936E-16,-1.));
#3672=DIRECTION('',(0.,1.,0.));
#3673=DIRECTION('',(0.,0.,1.));
#3674=DIRECTION('center_axis',(1.,0.,0.));
#3675=DIRECTION('ref_axis',(0.,0.,-1.));
#3676=DIRECTION('',(0.,1.,4.88654500275157E-16));
#3677=DIRECTION('center_axis',(1.,0.,0.));
#3678=DIRECTION('ref_axis',(0.,0.,-1.));
#3679=DIRECTION('',(0.,-4.88654500275157E-16,1.));
#3680=DIRECTION('',(0.,1.,0.));
#3681=DIRECTION('',(0.,-5.78241158658936E-16,1.));
#3682=DIRECTION('center_axis',(1.,0.,0.));
#3683=DIRECTION('ref_axis',(0.,0.,-1.));
#3684=DIRECTION('',(0.,-1.,-5.78241158658936E-16));
#3685=DIRECTION('center_axis',(1.,0.,0.));
#3686=DIRECTION('ref_axis',(0.,0.,-1.));
#3687=DIRECTION('center_axis',(-1.4960729241273E-31,-1.,-4.88654500275157E-16));
#3688=DIRECTION('ref_axis',(9.30044539122197E-64,4.88654500275157E-16,-1.));
#3689=DIRECTION('',(1.,-1.4960729241273E-31,0.));
#3690=DIRECTION('',(-2.8256014442301E-31,4.88654500275157E-16,-1.));
#3691=DIRECTION('',(1.,-1.4960729241273E-31,0.));
#3692=DIRECTION('',(1.,0.,-3.06161699786839E-16));
#3693=DIRECTION('',(-1.22464679914735E-16,4.88654500275157E-16,-1.));
#3694=DIRECTION('',(-1.,1.4960729241273E-31,0.));
#3695=DIRECTION('',(2.8256014442301E-31,4.88654500275157E-16,-1.));
#3696=DIRECTION('',(-1.,1.4960729241273E-31,0.));
#3697=DIRECTION('',(-1.22464679914735E-16,4.88654500275157E-16,-1.));
#3698=DIRECTION('',(1.,0.,-3.06161699786839E-16));
#3699=DIRECTION('',(0.,-4.88654500275157E-16,1.));
#3700=DIRECTION('center_axis',(0.,1.,0.));
#3701=DIRECTION('ref_axis',(0.,0.,1.));
#3702=DIRECTION('',(-1.,0.,0.));
#3703=DIRECTION('',(0.,0.,1.));
#3704=DIRECTION('',(1.,0.,-3.06161699786839E-16));
#3705=DIRECTION('',(-1.22464679914735E-16,0.,-1.));
#3706=DIRECTION('',(1.,0.,0.));
#3707=DIRECTION('',(0.,0.,1.));
#3708=DIRECTION('',(1.,0.,0.));
#3709=DIRECTION('',(-1.22464679914735E-16,0.,-1.));
#3710=DIRECTION('',(1.,0.,-3.06161699786839E-16));
#3711=DIRECTION('',(-1.,0.,0.));
#3712=DIRECTION('',(0.,0.,1.));
#3713=DIRECTION('center_axis',(-1.,0.,1.22464679914735E-16));
#3714=DIRECTION('ref_axis',(0.,-1.,0.));
#3715=DIRECTION('',(0.,1.,0.));
#3716=DIRECTION('',(-1.22464679914735E-16,5.78241158658936E-16,-1.));
#3717=DIRECTION('center_axis',(-1.,0.,1.22464679914735E-16));
#3718=DIRECTION('ref_axis',(1.22464679914735E-16,0.,1.));
#3719=DIRECTION('',(-7.08141184086923E-32,-1.,-5.78241158658936E-16));
#3720=DIRECTION('center_axis',(-1.,0.,1.22464679914735E-16));
#3721=DIRECTION('ref_axis',(1.22464679914735E-16,0.,1.));
#3722=DIRECTION('',(1.22464679914735E-16,-5.78241158658936E-16,1.));
#3723=DIRECTION('',(0.,1.,0.));
#3724=DIRECTION('center_axis',(-1.,0.,1.22464679914735E-16));
#3725=DIRECTION('ref_axis',(1.22464679914735E-16,0.,1.));
#3726=DIRECTION('',(-5.9842916965092E-32,-1.,-4.88654500275157E-16));
#3727=DIRECTION('center_axis',(-1.,0.,1.22464679914735E-16));
#3728=DIRECTION('ref_axis',(1.22464679914735E-16,0.,1.));
#3729=DIRECTION('center_axis',(1.77035296021731E-31,1.,5.78241158658936E-16));
#3730=DIRECTION('ref_axis',(6.82567686290692E-63,-5.78241158658936E-16,
1.));
#3731=DIRECTION('',(-1.,1.77035296021731E-31,0.));
#3732=DIRECTION('',(0.,-5.78241158658936E-16,1.));
#3733=DIRECTION('',(1.,0.,-3.06161699786839E-16));
#3734=DIRECTION('',(1.,-1.77035296021731E-31,0.));
#3735=DIRECTION('',(-3.34362837567229E-31,-5.78241158658936E-16,1.));
#3736=DIRECTION('',(1.,-1.77035296021731E-31,0.));
#3737=DIRECTION('',(-1.22464679914735E-16,5.78241158658936E-16,-1.));
#3738=DIRECTION('',(1.,0.,-3.06161699786839E-16));
#3739=DIRECTION('',(-1.,1.77035296021731E-31,0.));
#3740=DIRECTION('',(3.34362837567229E-31,-5.78241158658936E-16,1.));
#3741=DIRECTION('center_axis',(-1.77035296021731E-31,-1.,-5.78241158658936E-16));
#3742=DIRECTION('ref_axis',(-6.82567686290692E-63,5.78241158658936E-16,
-1.));
#3743=DIRECTION('',(1.,-1.77035296021731E-31,0.));
#3744=DIRECTION('',(-3.34362837567229E-31,5.78241158658936E-16,-1.));
#3745=DIRECTION('',(1.,-1.77035296021731E-31,0.));
#3746=DIRECTION('',(1.,0.,-3.06161699786839E-16));
#3747=DIRECTION('',(1.22464679914735E-16,-5.78241158658936E-16,1.));
#3748=DIRECTION('',(-1.,1.77035296021731E-31,0.));
#3749=DIRECTION('',(3.34362837567229E-31,5.78241158658936E-16,-1.));
#3750=DIRECTION('',(-1.,1.77035296021731E-31,0.));
#3751=DIRECTION('',(1.,0.,-3.06161699786839E-16));
#3752=DIRECTION('',(0.,5.78241158658936E-16,-1.));
#3753=DIRECTION('center_axis',(-3.06161699786839E-16,5.78241158658936E-16,
-1.));
#3754=DIRECTION('ref_axis',(0.,1.,5.78241158658936E-16));
#3755=DIRECTION('',(0.,1.,5.78241158658936E-16));
#3756=DIRECTION('',(1.,0.,-3.06161699786839E-16));
#3757=DIRECTION('',(1.,0.,-3.06161699786839E-16));
#3758=DIRECTION('center_axis',(1.,0.,-3.06161699786839E-16));
#3759=DIRECTION('ref_axis',(-3.06161699786839E-16,0.,-1.));
#3760=DIRECTION('center_axis',(1.,0.,0.));
#3761=DIRECTION('ref_axis',(0.,0.,-1.));
#3762=DIRECTION('center_axis',(1.,0.,-3.06161699786839E-16));
#3763=DIRECTION('ref_axis',(-3.06161699786839E-16,0.,-1.));
#3764=DIRECTION('',(1.,0.,-3.06161699786839E-16));
#3765=DIRECTION('center_axis',(-1.,0.,1.22464679914735E-16));
#3766=DIRECTION('ref_axis',(1.22464679914735E-16,0.,1.));
#3767=DIRECTION('center_axis',(3.06161699786839E-16,-5.78241158658936E-16,
1.));
#3768=DIRECTION('ref_axis',(0.,-1.,-5.78241158658936E-16));
#3769=DIRECTION('',(1.,0.,-3.06161699786839E-16));
#3770=DIRECTION('',(7.08141184086923E-32,1.,5.78241158658936E-16));
#3771=DIRECTION('',(1.,1.77035296021731E-31,-3.06161699786839E-16));
#3772=DIRECTION('',(1.77035296021731E-31,1.,5.78241158658936E-16));
#3773=DIRECTION('',(1.,1.77035296021731E-31,-3.06161699786839E-16));
#3774=DIRECTION('',(1.77035296021731E-31,1.,5.78241158658936E-16));
#3775=DIRECTION('center_axis',(1.,0.,-3.06161699786839E-16));
#3776=DIRECTION('ref_axis',(-3.06161699786839E-16,0.,-1.));
#3777=DIRECTION('center_axis',(-1.,0.,1.22464679914735E-16));
#3778=DIRECTION('ref_axis',(1.22464679914735E-16,0.,1.));
#3779=DIRECTION('center_axis',(1.,0.,-3.06161699786839E-16));
#3780=DIRECTION('ref_axis',(-3.06161699786839E-16,0.,-1.));
#3781=DIRECTION('center_axis',(1.,0.,0.));
#3782=DIRECTION('ref_axis',(0.,0.,-1.));
#3783=DIRECTION('center_axis',(1.,0.,0.));
#3784=DIRECTION('ref_axis',(0.,1.,0.));
#3785=DIRECTION('',(0.,1.,0.));
#3786=DIRECTION('',(0.,1.,0.));
#3787=DIRECTION('center_axis',(1.,0.,0.));
#3788=DIRECTION('ref_axis',(0.,0.,-1.));
#3789=DIRECTION('',(0.,1.,4.88654500275157E-16));
#3790=DIRECTION('center_axis',(1.,0.,0.));
#3791=DIRECTION('ref_axis',(0.,0.,-1.));
#3792=DIRECTION('center_axis',(-1.,0.,1.22464679914735E-16));
#3793=DIRECTION('ref_axis',(0.,-1.,0.));
#3794=DIRECTION('',(0.,1.,0.));
#3795=DIRECTION('center_axis',(-1.,0.,1.22464679914735E-16));
#3796=DIRECTION('ref_axis',(1.22464679914735E-16,0.,1.));
#3797=DIRECTION('',(-5.98429169650921E-32,-1.,-4.88654500275157E-16));
#3798=DIRECTION('center_axis',(-1.,0.,1.22464679914735E-16));
#3799=DIRECTION('ref_axis',(1.22464679914735E-16,0.,1.));
#3800=DIRECTION('',(0.,1.,0.));
#3801=DIRECTION('center_axis',(1.,0.,-3.06161699786839E-16));
#3802=DIRECTION('ref_axis',(-3.06161699786839E-16,0.,-1.));
#3803=DIRECTION('',(1.,0.,-3.06161699786839E-16));
#3804=DIRECTION('center_axis',(1.,0.,-3.06161699786839E-16));
#3805=DIRECTION('ref_axis',(-3.06161699786839E-16,0.,-1.));
#3806=DIRECTION('',(1.,0.,-3.06161699786839E-16));
#3807=DIRECTION('center_axis',(3.06161699786839E-16,-4.88654500275157E-16,
1.));
#3808=DIRECTION('ref_axis',(0.,-1.,-4.88654500275157E-16));
#3809=DIRECTION('',(1.,0.,-3.06161699786839E-16));
#3810=DIRECTION('center_axis',(1.,0.,-3.06161699786839E-16));
#3811=DIRECTION('ref_axis',(-3.06161699786839E-16,0.,-1.));
#3812=DIRECTION('center_axis',(1.,0.,-3.06161699786839E-16));
#3813=DIRECTION('ref_axis',(-3.06161699786839E-16,0.,-1.));
#3814=DIRECTION('',(1.,0.,-3.06161699786839E-16));
#3815=DIRECTION('center_axis',(-3.06161699786839E-16,4.88654500275157E-16,
-1.));
#3816=DIRECTION('ref_axis',(0.,1.,4.88654500275157E-16));
#3817=DIRECTION('',(-1.,-1.77035296021731E-31,3.06161699786839E-16));
#3818=DIRECTION('',(-1.4960729241273E-31,-1.,-4.88654500275157E-16));
#3819=DIRECTION('',(-1.,-1.77035296021731E-31,3.06161699786839E-16));
#3820=DIRECTION('',(-1.4960729241273E-31,-1.,-4.88654500275157E-16));
#3821=DIRECTION('center_axis',(0.,0.,1.));
#3822=DIRECTION('ref_axis',(1.,0.,0.));
#3823=DIRECTION('',(-5.78241158658936E-16,-1.,0.));
#3824=DIRECTION('center_axis',(-1.,5.78241158658936E-16,0.));
#3825=DIRECTION('ref_axis',(-5.78241158658936E-16,-1.,0.));
#3826=DIRECTION('',(-5.78241158658936E-16,-1.,0.));
#3827=DIRECTION('center_axis',(0.,0.,1.));
#3828=DIRECTION('ref_axis',(1.,0.,0.));
#3829=DIRECTION('center_axis',(0.,0.,1.));
#3830=DIRECTION('ref_axis',(1.,0.,0.));
#3831=DIRECTION('',(-5.78241158658936E-16,-1.,0.));
#3832=DIRECTION('center_axis',(-1.,5.78241158658936E-16,0.));
#3833=DIRECTION('ref_axis',(-5.78241158658936E-16,-1.,0.));
#3834=DIRECTION('',(-5.78241158658936E-16,-1.,0.));
#3835=DIRECTION('center_axis',(0.,0.,1.));
#3836=DIRECTION('ref_axis',(1.,0.,0.));
#3837=DIRECTION('center_axis',(0.,0.,-1.));
#3838=DIRECTION('ref_axis',(-1.,0.,0.));
#3839=DIRECTION('',(5.78241158658936E-16,-1.,0.));
#3840=DIRECTION('center_axis',(0.,0.,-1.));
#3841=DIRECTION('ref_axis',(-1.,0.,0.));
#3842=DIRECTION('',(5.78241158658936E-16,-1.,0.));
#3843=DIRECTION('center_axis',(-1.,-5.78241158658936E-16,0.));
#3844=DIRECTION('ref_axis',(5.78241158658936E-16,-1.,0.));
#3845=DIRECTION('center_axis',(0.,0.,-1.));
#3846=DIRECTION('ref_axis',(-1.,0.,0.));
#3847=DIRECTION('',(5.78241158658936E-16,-1.,0.));
#3848=DIRECTION('center_axis',(0.,0.,-1.));
#3849=DIRECTION('ref_axis',(-1.,0.,0.));
#3850=DIRECTION('',(5.78241158658936E-16,-1.,0.));
#3851=DIRECTION('center_axis',(-1.,-5.78241158658936E-16,0.));
#3852=DIRECTION('ref_axis',(5.78241158658936E-16,-1.,0.));
#3853=DIRECTION('center_axis',(0.,-1.,-5.78241158658936E-16));
#3854=DIRECTION('ref_axis',(0.,5.78241158658936E-16,-1.));
#3855=DIRECTION('',(3.06161699786839E-16,-5.78241158658936E-16,1.));
#3856=DIRECTION('',(3.06161699786839E-16,-5.78241158658936E-16,1.));
#3857=DIRECTION('center_axis',(1.,-2.73691106313441E-47,-3.06161699786839E-16));
#3858=DIRECTION('ref_axis',(-3.06161699786839E-16,0.,-1.));
#3859=DIRECTION('',(3.06161699786839E-16,-5.78241158658936E-16,1.));
#3860=DIRECTION('center_axis',(0.,-1.,-5.78241158658936E-16));
#3861=DIRECTION('ref_axis',(0.,5.78241158658936E-16,-1.));
#3862=DIRECTION('',(3.06161699786839E-16,-5.78241158658936E-16,1.));
#3863=DIRECTION('center_axis',(1.,-2.73691106313441E-47,-3.06161699786839E-16));
#3864=DIRECTION('ref_axis',(-3.06161699786839E-16,0.,-1.));
#3865=DIRECTION('axis',(0.,0.,1.));
#3866=DIRECTION('refdir',(1.,0.,0.));
#3867=DIRECTION('center_axis',(-2.28847549044393E-17,-4.88654500275157E-16,
-1.));
#3868=DIRECTION('ref_axis',(0.,1.,-4.88654500275157E-16));
#3869=DIRECTION('',(-1.,-1.22464679914735E-16,2.28847549044394E-17));
#3870=DIRECTION('',(-1.22464679914735E-16,1.,-4.88654500275157E-16));
#3871=DIRECTION('',(-1.,-1.22464679914735E-16,2.28847549044394E-17));
#3872=DIRECTION('',(-1.22464679914735E-16,1.,-4.88654500275157E-16));
#3873=DIRECTION('',(-1.,1.32329071915688E-32,2.28847549044393E-17));
#3874=DIRECTION('',(-1.11827384717482E-32,1.,-4.88654500275157E-16));
#3875=DIRECTION('',(-1.,1.32329071915688E-32,2.28847549044393E-17));
#3876=DIRECTION('',(-1.11827384717482E-32,1.,-4.88654500275157E-16));
#3877=DIRECTION('',(1.,-1.32329071915688E-32,-2.28847549044393E-17));
#3878=DIRECTION('',(-1.11827384717482E-32,1.,-4.88654500275157E-16));
#3879=DIRECTION('',(1.,-1.32329071915688E-32,-2.28847549044393E-17));
#3880=DIRECTION('',(-1.11827384717482E-32,1.,-4.88654500275157E-16));
#3881=DIRECTION('center_axis',(2.28847549044393E-17,5.78241158658936E-16,
1.));
#3882=DIRECTION('ref_axis',(0.,-1.,5.78241158658936E-16));
#3883=DIRECTION('',(-1.,-1.22464679914735E-16,2.28847549044394E-17));
#3884=DIRECTION('',(-1.22464679914735E-16,1.,-5.78241158658936E-16));
#3885=DIRECTION('',(-1.,-1.22464679914735E-16,2.28847549044394E-17));
#3886=DIRECTION('',(-1.22464679914735E-16,1.,-5.78241158658936E-16));
#3887=DIRECTION('',(1.,-1.32329071915687E-32,-2.28847549044393E-17));
#3888=DIRECTION('',(1.32329071915687E-32,-1.,5.78241158658936E-16));
#3889=DIRECTION('',(1.,-1.32329071915687E-32,-2.28847549044393E-17));
#3890=DIRECTION('',(1.32329071915687E-32,-1.,5.78241158658936E-16));
#3891=DIRECTION('',(-1.,1.32329071915687E-32,2.28847549044393E-17));
#3892=DIRECTION('',(1.32329071915687E-32,-1.,5.78241158658936E-16));
#3893=DIRECTION('',(-1.,1.32329071915687E-32,2.28847549044393E-17));
#3894=DIRECTION('',(1.32329071915687E-32,-1.,5.78241158658936E-16));
#3895=DIRECTION('center_axis',(-1.710569414459E-48,-1.,5.78241158658936E-16));
#3896=DIRECTION('ref_axis',(1.82731431016009E-80,-5.78241158658936E-16,
-1.));
#3897=DIRECTION('',(2.28847549044393E-17,-5.78241158658936E-16,-1.));
#3898=DIRECTION('',(-1.,-1.32329071915688E-32,-2.28847549044394E-17));
#3899=DIRECTION('',(2.28847549044393E-17,-5.78241158658936E-16,-1.));
#3900=DIRECTION('',(1.,1.32329071915687E-32,2.28847549044393E-17));
#3901=DIRECTION('center_axis',(1.,1.710569414459E-48,2.28847549044393E-17));
#3902=DIRECTION('ref_axis',(-2.28847549044393E-17,0.,1.));
#3903=DIRECTION('',(1.64643319114981E-48,-1.,2.80257418429934E-33));
#3904=DIRECTION('',(2.28847549044393E-17,-5.78241158658936E-16,-1.));
#3905=DIRECTION('',(1.32329071915687E-32,1.,-5.78241158658936E-16));
#3906=DIRECTION('center_axis',(1.710569414459E-48,1.,-5.78241158658936E-16));
#3907=DIRECTION('ref_axis',(-1.82731431016009E-80,5.78241158658936E-16,
1.));
#3908=DIRECTION('',(1.,1.32329071915688E-32,2.28847549044394E-17));
#3909=DIRECTION('',(2.28847549044393E-17,-5.78241158658936E-16,-1.));
#3910=DIRECTION('',(-1.,-1.32329071915687E-32,-2.28847549044393E-17));
#3911=DIRECTION('center_axis',(-1.,-1.710569414459E-48,-2.28847549044393E-17));
#3912=DIRECTION('ref_axis',(2.28847549044393E-17,0.,-1.));
#3913=DIRECTION('',(-1.64643319114981E-48,1.,-2.80257418429934E-33));
#3914=DIRECTION('',(-1.32329071915687E-32,-1.,5.78241158658936E-16));
#3915=DIRECTION('center_axis',(-1.710569414459E-48,-1.,5.78241158658936E-16));
#3916=DIRECTION('ref_axis',(1.82731431016009E-80,-5.78241158658936E-16,
-1.));
#3917=DIRECTION('',(2.28847549044393E-17,-5.78241158658936E-16,-1.));
#3918=DIRECTION('',(-1.,-1.32329071915688E-32,-2.28847549044394E-17));
#3919=DIRECTION('',(2.28847549044393E-17,-5.78241158658936E-16,-1.));
#3920=DIRECTION('',(1.,1.32329071915687E-32,2.28847549044393E-17));
#3921=DIRECTION('center_axis',(-1.,-1.710569414459E-48,-2.28847549044393E-17));
#3922=DIRECTION('ref_axis',(2.28847549044393E-17,0.,-1.));
#3923=DIRECTION('',(-1.64643319114981E-48,1.,-2.80257418429934E-33));
#3924=DIRECTION('',(2.28847549044393E-17,-5.78241158658936E-16,-1.));
#3925=DIRECTION('',(-1.32329071915687E-32,-1.,5.78241158658936E-16));
#3926=DIRECTION('center_axis',(-1.710569414459E-48,-1.,5.78241158658936E-16));
#3927=DIRECTION('ref_axis',(1.82731431016009E-80,-5.78241158658936E-16,
-1.));
#3928=DIRECTION('',(-1.,-1.32329071915688E-32,-2.28847549044394E-17));
#3929=DIRECTION('',(2.28847549044393E-17,-5.78241158658936E-16,-1.));
#3930=DIRECTION('',(1.,1.32329071915687E-32,2.28847549044393E-17));
#3931=DIRECTION('center_axis',(-1.,-1.710569414459E-48,-2.28847549044393E-17));
#3932=DIRECTION('ref_axis',(2.28847549044393E-17,0.,-1.));
#3933=DIRECTION('',(-1.64643319114981E-48,1.,-2.80257418429934E-33));
#3934=DIRECTION('',(-1.32329071915687E-32,-1.,5.78241158658936E-16));
#3935=DIRECTION('center_axis',(2.28847549044394E-17,2.80257418429934E-33,
1.));
#3936=DIRECTION('ref_axis',(1.,4.56206030093224E-66,-2.28847549044394E-17));
#3937=DIRECTION('',(-1.,-1.22464679914735E-16,2.28847549044394E-17));
#3938=DIRECTION('',(-1.22464679914735E-16,1.,0.));
#3939=DIRECTION('',(-1.,-1.22464679914735E-16,2.28847549044394E-17));
#3940=DIRECTION('',(-1.22464679914735E-16,1.,0.));
#3941=DIRECTION('',(-1.,1.32329071915688E-32,2.28847549044394E-17));
#3942=DIRECTION('',(1.64643319114981E-48,1.,-2.80257418429934E-33));
#3943=DIRECTION('',(1.,-1.32329071915688E-32,-2.28847549044394E-17));
#3944=DIRECTION('',(-1.64643319114981E-48,-1.,2.80257418429934E-33));
#3945=DIRECTION('',(1.,-1.32329071915688E-32,-2.28847549044394E-17));
#3946=DIRECTION('',(1.64643319114981E-48,1.,-2.80257418429934E-33));
#3947=DIRECTION('',(1.,-1.32329071915688E-32,-2.28847549044394E-17));
#3948=DIRECTION('',(1.64643319114981E-48,1.,-2.80257418429934E-33));
#3949=DIRECTION('center_axis',(-2.28847549044393E-17,-5.78241158658936E-16,
-1.));
#3950=DIRECTION('ref_axis',(0.,1.,-5.78241158658936E-16));
#3951=DIRECTION('',(-1.,-1.22464679914735E-16,2.28847549044394E-17));
#3952=DIRECTION('',(-1.22464679914735E-16,1.,-5.78241158658936E-16));
#3953=DIRECTION('',(-1.,-1.22464679914735E-16,2.28847549044394E-17));
#3954=DIRECTION('',(-1.22464679914735E-16,1.,-5.78241158658936E-16));
#3955=DIRECTION('',(-1.,1.32329071915687E-32,2.28847549044393E-17));
#3956=DIRECTION('',(1.32329071915687E-32,-1.,5.78241158658936E-16));
#3957=DIRECTION('',(1.,-1.32329071915687E-32,-2.28847549044393E-17));
#3958=DIRECTION('',(-1.32329071915687E-32,1.,-5.78241158658936E-16));
#3959=DIRECTION('',(-1.,1.32329071915687E-32,2.28847549044393E-17));
#3960=DIRECTION('',(1.32329071915687E-32,-1.,5.78241158658936E-16));
#3961=DIRECTION('',(-1.,1.32329071915687E-32,2.28847549044393E-17));
#3962=DIRECTION('',(1.32329071915687E-32,-1.,5.78241158658936E-16));
#3963=DIRECTION('center_axis',(1.22464679914735E-16,-1.,5.78241158658936E-16));
#3964=DIRECTION('ref_axis',(1.41228329145101E-48,-5.78241158658936E-16,
-1.));
#3965=DIRECTION('',(2.28847549044393E-17,5.78241158658936E-16,1.));
#3966=DIRECTION('',(-1.,-1.22464679914735E-16,2.28847549044394E-17));
#3967=DIRECTION('',(2.28847549044393E-17,5.78241158658936E-16,1.));
#3968=DIRECTION('',(-1.,-1.22464679914735E-16,2.28847549044394E-17));
#3969=DIRECTION('center_axis',(-1.,-1.22464679914735E-16,2.28847549044394E-17));
#3970=DIRECTION('ref_axis',(1.22464679914735E-16,-1.,-1.1877739243467E-49));
#3971=DIRECTION('center_axis',(-1.,-1.22464679914735E-16,2.28847549044394E-17));
#3972=DIRECTION('ref_axis',(-2.28847549044394E-17,-2.80257418429934E-33,
-1.));
#3973=DIRECTION('center_axis',(-1.,-1.22464679914735E-16,2.28847549044394E-17));
#3974=DIRECTION('ref_axis',(-2.28847549044394E-17,-2.80257418429934E-33,
-1.));
#3975=DIRECTION('center_axis',(-1.,-1.22464679914735E-16,2.28847549044394E-17));
#3976=DIRECTION('ref_axis',(1.22464679914735E-16,-1.,-1.1877739243467E-49));
#3977=DIRECTION('center_axis',(-1.,-1.22464679914735E-16,2.28847549044394E-17));
#3978=DIRECTION('ref_axis',(-2.28847549044394E-17,-2.80257418429934E-33,
-1.));
#3979=DIRECTION('',(-1.,-1.22464679914735E-16,2.28847549044394E-17));
#3980=DIRECTION('center_axis',(-1.,-1.22464679914735E-16,2.28847549044394E-17));
#3981=DIRECTION('ref_axis',(-2.28847549044394E-17,-2.80257418429934E-33,
-1.));
#3982=DIRECTION('center_axis',(-1.22464679914735E-16,1.,-5.78241158658936E-16));
#3983=DIRECTION('ref_axis',(-1.41228329145101E-48,5.78241158658936E-16,
1.));
#3984=DIRECTION('',(2.28847549044393E-17,5.78241158658936E-16,1.));
#3985=DIRECTION('',(-1.,-1.22464679914735E-16,2.28847549044394E-17));
#3986=DIRECTION('',(2.28847549044393E-17,5.78241158658936E-16,1.));
#3987=DIRECTION('center_axis',(-1.,-1.22464679914735E-16,2.28847549044394E-17));
#3988=DIRECTION('ref_axis',(1.22464679914735E-16,-1.,-1.1877739243467E-49));
#3989=DIRECTION('center_axis',(-1.,-1.22464679914735E-16,2.28847549044394E-17));
#3990=DIRECTION('ref_axis',(-2.28847549044394E-17,-2.80257418429934E-33,
-1.));
#3991=DIRECTION('center_axis',(-1.,-1.22464679914735E-16,2.28847549044394E-17));
#3992=DIRECTION('ref_axis',(-2.28847549044394E-17,-2.80257418429934E-33,
-1.));
#3993=DIRECTION('center_axis',(-1.,-1.22464679914735E-16,2.28847549044394E-17));
#3994=DIRECTION('ref_axis',(1.22464679914735E-16,-1.,-1.1877739243467E-49));
#3995=DIRECTION('center_axis',(-1.,-1.22464679914735E-16,2.28847549044394E-17));
#3996=DIRECTION('ref_axis',(-2.28847549044394E-17,-2.80257418429934E-33,
-1.));
#3997=DIRECTION('center_axis',(-1.,-1.22464679914735E-16,2.28847549044394E-17));
#3998=DIRECTION('ref_axis',(-2.28847549044394E-17,-2.80257418429934E-33,
-1.));
#3999=DIRECTION('center_axis',(-1.,-1.22464679914735E-16,2.28847549044394E-17));
#4000=DIRECTION('ref_axis',(1.22464679914735E-16,-1.,-1.1877739243467E-49));
#4001=DIRECTION('center_axis',(-1.,-1.22464679914735E-16,2.28847549044394E-17));
#4002=DIRECTION('ref_axis',(-2.28847549044394E-17,-2.80257418429934E-33,
-1.));
#4003=DIRECTION('center_axis',(-1.,-1.22464679914735E-16,2.28847549044394E-17));
#4004=DIRECTION('ref_axis',(-2.28847549044394E-17,-2.80257418429934E-33,
-1.));
#4005=DIRECTION('',(2.28847549044393E-17,4.88654500275157E-16,1.));
#4006=DIRECTION('center_axis',(-1.,-1.22464679914735E-16,2.28847549044394E-17));
#4007=DIRECTION('ref_axis',(-2.28847549044394E-17,-2.80257418429934E-33,
-1.));
#4008=DIRECTION('center_axis',(-1.,-1.22464679914735E-16,2.28847549044394E-17));
#4009=DIRECTION('ref_axis',(-2.28847549044394E-17,-2.80257418429934E-33,
-1.));
#4010=DIRECTION('',(2.28847549044393E-17,4.88654500275157E-16,1.));
#4011=DIRECTION('center_axis',(-1.,-1.22464679914735E-16,2.28847549044394E-17));
#4012=DIRECTION('ref_axis',(1.22464679914735E-16,-1.,-1.1877739243467E-49));
#4013=DIRECTION('center_axis',(-1.,-1.22464679914735E-16,2.28847549044394E-17));
#4014=DIRECTION('ref_axis',(-2.28847549044394E-17,-2.80257418429934E-33,
-1.));
#4015=DIRECTION('',(2.28847549044393E-17,4.88654500275157E-16,1.));
#4016=DIRECTION('center_axis',(-1.,-1.22464679914735E-16,2.28847549044394E-17));
#4017=DIRECTION('ref_axis',(-2.28847549044394E-17,-2.80257418429934E-33,
-1.));
#4018=DIRECTION('center_axis',(-1.,-1.22464679914735E-16,2.28847549044394E-17));
#4019=DIRECTION('ref_axis',(-2.28847549044394E-17,-2.80257418429934E-33,
-1.));
#4020=DIRECTION('',(2.28847549044393E-17,4.88654500275157E-16,1.));
#4021=DIRECTION('center_axis',(-1.,-1.22464679914735E-16,2.28847549044394E-17));
#4022=DIRECTION('ref_axis',(-2.28847549044394E-17,-2.80257418429934E-33,
-1.));
#4023=DIRECTION('center_axis',(-1.,-1.22464679914735E-16,2.28847549044394E-17));
#4024=DIRECTION('ref_axis',(1.22464679914735E-16,-1.,-1.1877739243467E-49));
#4025=DIRECTION('',(-1.,-1.22464679914735E-16,2.28847549044394E-17));
#4026=DIRECTION('center_axis',(-1.,-1.22464679914735E-16,2.28847549044394E-17));
#4027=DIRECTION('ref_axis',(1.22464679914735E-16,-1.,-1.1877739243467E-49));
#4028=DIRECTION('',(-1.,-1.22464679914735E-16,2.28847549044394E-17));
#4029=DIRECTION('center_axis',(-1.22464679914735E-16,1.,-4.88654500275157E-16));
#4030=DIRECTION('ref_axis',(-3.23663765428249E-48,4.88654500275157E-16,
1.));
#4031=DIRECTION('',(-1.,-1.22464679914735E-16,2.28847549044394E-17));
#4032=DIRECTION('center_axis',(-1.,-1.22464679914735E-16,2.28847549044394E-17));
#4033=DIRECTION('ref_axis',(1.22464679914735E-16,-1.,-1.1877739243467E-49));
#4034=DIRECTION('center_axis',(-1.,-1.22464679914735E-16,2.28847549044394E-17));
#4035=DIRECTION('ref_axis',(1.22464679914735E-16,-1.,-1.1877739243467E-49));
#4036=DIRECTION('',(-1.,-1.22464679914735E-16,2.28847549044394E-17));
#4037=DIRECTION('center_axis',(1.22464679914735E-16,-1.,4.88654500275157E-16));
#4038=DIRECTION('ref_axis',(3.23663765428249E-48,-4.88654500275157E-16,
-1.));
#4039=DIRECTION('center_axis',(1.,-1.710569414459E-48,-2.28847549044393E-17));
#4040=DIRECTION('ref_axis',(-2.28847549044393E-17,0.,-1.));
#4041=DIRECTION('',(-2.28847549044393E-17,-5.78241158658936E-16,-1.));
#4042=DIRECTION('',(-2.28847549044393E-17,-5.78241158658936E-16,-1.));
#4043=DIRECTION('center_axis',(1.710569414459E-48,-1.,5.78241158658936E-16));
#4044=DIRECTION('ref_axis',(-1.82731431016009E-80,-5.78241158658936E-16,
-1.));
#4045=DIRECTION('',(-2.28847549044393E-17,-5.78241158658936E-16,-1.));
#4046=DIRECTION('center_axis',(-1.,1.710569414459E-48,2.28847549044393E-17));
#4047=DIRECTION('ref_axis',(2.28847549044393E-17,0.,1.));
#4048=DIRECTION('',(-2.28847549044393E-17,-5.78241158658936E-16,-1.));
#4049=DIRECTION('center_axis',(-1.710569414459E-48,1.,-5.78241158658936E-16));
#4050=DIRECTION('ref_axis',(1.82731431016009E-80,5.78241158658936E-16,1.));
#4051=DIRECTION('center_axis',(1.,-1.710569414459E-48,-2.28847549044393E-17));
#4052=DIRECTION('ref_axis',(-2.28847549044393E-17,0.,-1.));
#4053=DIRECTION('',(-2.28847549044393E-17,-5.78241158658936E-16,-1.));
#4054=DIRECTION('',(-2.28847549044393E-17,-5.78241158658936E-16,-1.));
#4055=DIRECTION('center_axis',(1.710569414459E-48,-1.,5.78241158658936E-16));
#4056=DIRECTION('ref_axis',(-1.82731431016009E-80,-5.78241158658936E-16,
-1.));
#4057=DIRECTION('',(-2.28847549044393E-17,-5.78241158658936E-16,-1.));
#4058=DIRECTION('center_axis',(1.,-1.710569414459E-48,-2.28847549044393E-17));
#4059=DIRECTION('ref_axis',(-2.28847549044393E-17,0.,-1.));
#4060=DIRECTION('',(-2.28847549044393E-17,-5.78241158658936E-16,-1.));
#4061=DIRECTION('center_axis',(1.710569414459E-48,-1.,5.78241158658936E-16));
#4062=DIRECTION('ref_axis',(-1.82731431016009E-80,-5.78241158658936E-16,
-1.));
#4063=DIRECTION('center_axis',(-1.,1.710569414459E-48,2.28847549044393E-17));
#4064=DIRECTION('ref_axis',(2.28847549044393E-17,0.,1.));
#4065=DIRECTION('',(2.28847549044393E-17,5.78241158658936E-16,1.));
#4066=DIRECTION('',(2.28847549044393E-17,5.78241158658936E-16,1.));
#4067=DIRECTION('center_axis',(1.710569414459E-48,-1.,5.78241158658936E-16));
#4068=DIRECTION('ref_axis',(-1.82731431016009E-80,-5.78241158658936E-16,
-1.));
#4069=DIRECTION('',(2.28847549044393E-17,5.78241158658936E-16,1.));
#4070=DIRECTION('center_axis',(-1.,1.710569414459E-48,2.28847549044393E-17));
#4071=DIRECTION('ref_axis',(2.28847549044393E-17,0.,1.));
#4072=DIRECTION('',(2.28847549044393E-17,5.78241158658936E-16,1.));
#4073=DIRECTION('center_axis',(1.710569414459E-48,-1.,5.78241158658936E-16));
#4074=DIRECTION('ref_axis',(-1.82731431016009E-80,-5.78241158658936E-16,
-1.));
#4075=DIRECTION('center_axis',(-1.,1.710569414459E-48,2.28847549044393E-17));
#4076=DIRECTION('ref_axis',(2.28847549044393E-17,0.,1.));
#4077=DIRECTION('',(2.28847549044393E-17,5.78241158658936E-16,1.));
#4078=DIRECTION('',(2.28847549044393E-17,5.78241158658936E-16,1.));
#4079=DIRECTION('center_axis',(-1.710569414459E-48,1.,-5.78241158658936E-16));
#4080=DIRECTION('ref_axis',(1.82731431016009E-80,5.78241158658936E-16,1.));
#4081=DIRECTION('',(2.28847549044393E-17,5.78241158658936E-16,1.));
#4082=DIRECTION('center_axis',(-1.,1.710569414459E-48,2.28847549044393E-17));
#4083=DIRECTION('ref_axis',(2.28847549044393E-17,0.,1.));
#4084=DIRECTION('',(2.28847549044393E-17,5.78241158658936E-16,1.));
#4085=DIRECTION('center_axis',(-1.710569414459E-48,1.,-5.78241158658936E-16));
#4086=DIRECTION('ref_axis',(1.82731431016009E-80,5.78241158658936E-16,1.));
#4087=DIRECTION('axis',(0.,0.,1.));
#4088=DIRECTION('refdir',(1.,0.,0.));
#4089=DIRECTION('center_axis',(0.,0.,-1.));
#4090=DIRECTION('ref_axis',(-1.,0.,0.));
#4091=DIRECTION('center_axis',(0.,0.,-1.));
#4092=DIRECTION('ref_axis',(-1.,0.,0.));
#4093=DIRECTION('',(0.,0.,-1.));
#4094=DIRECTION('center_axis',(0.,0.,-1.));
#4095=DIRECTION('ref_axis',(-1.,0.,0.));
#4096=DIRECTION('center_axis',(0.,0.,1.));
#4097=DIRECTION('ref_axis',(1.,0.,0.));
#4098=DIRECTION('center_axis',(0.,0.,-1.));
#4099=DIRECTION('ref_axis',(-1.,0.,0.));
#4100=DIRECTION('center_axis',(0.,0.,-1.));
#4101=DIRECTION('ref_axis',(-1.,0.,0.));
#4102=DIRECTION('',(0.,0.,1.));
#4103=DIRECTION('center_axis',(0.,0.,-1.));
#4104=DIRECTION('ref_axis',(-1.,0.,0.));
#4105=DIRECTION('center_axis',(0.,0.,1.));
#4106=DIRECTION('ref_axis',(1.,0.,0.));
#4107=DIRECTION('center_axis',(0.,0.,-1.));
#4108=DIRECTION('ref_axis',(-1.,0.,0.));
#4109=DIRECTION('center_axis',(0.,0.,-1.));
#4110=DIRECTION('ref_axis',(-1.,0.,0.));
#4111=DIRECTION('center_axis',(0.,1.,0.));
#4112=DIRECTION('ref_axis',(1.,0.,0.));
#4113=DIRECTION('center_axis',(0.,0.,-1.));
#4114=DIRECTION('ref_axis',(-1.,0.,0.));
#4115=DIRECTION('center_axis',(0.,0.,1.));
#4116=DIRECTION('ref_axis',(1.,0.,0.));
#4117=DIRECTION('center_axis',(0.,0.,-1.));
#4118=DIRECTION('ref_axis',(-1.,0.,0.));
#4119=DIRECTION('center_axis',(0.,0.,-1.));
#4120=DIRECTION('ref_axis',(-1.,0.,0.));
#4121=DIRECTION('',(0.,0.,1.));
#4122=DIRECTION('center_axis',(0.,0.,-1.));
#4123=DIRECTION('ref_axis',(-1.,0.,0.));
#4124=DIRECTION('center_axis',(0.,0.,1.));
#4125=DIRECTION('ref_axis',(1.,0.,0.));
#4126=DIRECTION('axis',(0.,0.,1.));
#4127=DIRECTION('refdir',(1.,0.,0.));
#4128=DIRECTION('center_axis',(-1.,6.12618443423765E-16,1.10412253250333E-15));
#4129=DIRECTION('ref_axis',(1.10412253250334E-15,1.59865984135391E-14,1.));
#4130=DIRECTION('center_axis',(1.,-6.12618443423765E-16,-1.10412253250333E-15));
#4131=DIRECTION('ref_axis',(1.10412253250334E-15,1.59865984135391E-14,1.));
#4132=DIRECTION('center_axis',(-1.,0.,0.));
#4133=DIRECTION('ref_axis',(0.,1.59865984135391E-14,1.));
#4134=DIRECTION('center_axis',(-1.,6.12618443423765E-16,1.10412253250333E-15));
#4135=DIRECTION('ref_axis',(1.10412253250334E-15,1.59865984135391E-14,1.));
#4136=DIRECTION('',(1.,0.,0.));
#4137=DIRECTION('center_axis',(-1.,6.12618443423765E-16,1.10412253250333E-15));
#4138=DIRECTION('ref_axis',(1.10412253250334E-15,1.59865984135391E-14,1.));
#4139=DIRECTION('axis',(0.,0.,1.));
#4140=DIRECTION('refdir',(1.,0.,0.));
#4141=DIRECTION('center_axis',(-1.22464679914735E-16,0.,1.));
#4142=DIRECTION('ref_axis',(-1.,0.,-1.22464679914735E-16));
#4143=DIRECTION('',(-1.,1.32329071915687E-32,-2.28847549044393E-17));
#4144=DIRECTION('',(4.88654500275157E-16,1.,5.98429169650921E-32));
#4145=DIRECTION('center_axis',(1.22464679914735E-16,0.,-1.));
#4146=DIRECTION('ref_axis',(0.,-1.,0.));
#4147=DIRECTION('',(1.,-4.88654500275157E-16,1.22464679914735E-16));
#4148=DIRECTION('center_axis',(1.22464679914735E-16,0.,-1.));
#4149=DIRECTION('ref_axis',(0.,-1.,0.));
#4150=DIRECTION('',(4.88654500275157E-16,1.,5.9842916965092E-32));
#4151=DIRECTION('',(-1.,1.32329071915687E-32,-2.28847549044393E-17));
#4152=DIRECTION('',(5.78241158658936E-16,1.,7.08141184086923E-32));
#4153=DIRECTION('center_axis',(1.22464679914735E-16,0.,-1.));
#4154=DIRECTION('ref_axis',(0.,-1.,0.));
#4155=DIRECTION('',(1.,-5.78241158658936E-16,1.22464679914735E-16));
#4156=DIRECTION('center_axis',(1.22464679914735E-16,0.,-1.));
#4157=DIRECTION('ref_axis',(0.,-1.,0.));
#4158=DIRECTION('',(5.78241158658936E-16,1.,7.08141184086923E-32));
#4159=DIRECTION('center_axis',(-1.22464679914735E-16,0.,1.));
#4160=DIRECTION('ref_axis',(-1.,0.,-1.22464679914735E-16));
#4161=DIRECTION('',(5.78241158658936E-16,1.,7.08141184086923E-32));
#4162=DIRECTION('center_axis',(1.22464679914735E-16,0.,-1.));
#4163=DIRECTION('ref_axis',(0.,-1.,0.));
#4164=DIRECTION('',(1.,-5.78241158658936E-16,1.22464679914735E-16));
#4165=DIRECTION('center_axis',(1.22464679914735E-16,0.,-1.));
#4166=DIRECTION('ref_axis',(0.,-1.,0.));
#4167=DIRECTION('',(5.78241158658936E-16,1.,7.08141184086923E-32));
#4168=DIRECTION('',(-1.,1.32329071915687E-32,-2.28847549044393E-17));
#4169=DIRECTION('',(4.88654500275157E-16,1.,5.9842916965092E-32));
#4170=DIRECTION('center_axis',(1.22464679914735E-16,0.,-1.));
#4171=DIRECTION('ref_axis',(0.,-1.,0.));
#4172=DIRECTION('',(1.,0.,1.22464679914735E-16));
#4173=DIRECTION('center_axis',(1.22464679914735E-16,0.,-1.));
#4174=DIRECTION('ref_axis',(0.,-1.,0.));
#4175=DIRECTION('',(4.88654500275157E-16,1.,5.98429169650921E-32));
#4176=DIRECTION('',(-1.,1.32329071915687E-32,-2.28847549044393E-17));
#4177=DIRECTION('center_axis',(-5.78241158658936E-16,-1.,-7.08141184086922E-32));
#4178=DIRECTION('ref_axis',(1.,-5.78241158658936E-16,0.));
#4179=DIRECTION('',(-4.09476378780532E-47,-7.08141184086922E-32,1.));
#4180=DIRECTION('',(-1.,5.78241158658936E-16,4.09476378780532E-47));
#4181=DIRECTION('',(-1.22464679914735E-16,0.,1.));
#4182=DIRECTION('',(-1.22464679914735E-16,0.,1.));
#4183=DIRECTION('',(-1.,5.78241158658936E-16,-3.06161699786839E-16));
#4184=DIRECTION('',(-1.22464679914735E-16,0.,1.));
#4185=DIRECTION('',(-1.,5.78241158658936E-16,4.09476378780532E-47));
#4186=DIRECTION('center_axis',(-1.22464679914735E-16,0.,1.));
#4187=DIRECTION('ref_axis',(-1.,0.,-1.22464679914735E-16));
#4188=DIRECTION('center_axis',(3.06161699786839E-16,0.,-1.));
#4189=DIRECTION('ref_axis',(-1.,0.,-3.06161699786839E-16));
#4190=DIRECTION('',(-1.22464679914735E-16,0.,1.));
#4191=DIRECTION('center_axis',(0.,-7.08141184086922E-32,1.));
#4192=DIRECTION('ref_axis',(0.,-1.,-7.08141184086922E-32));
#4193=DIRECTION('center_axis',(-1.,5.78241158658936E-16,-1.22464679914735E-16));
#4194=DIRECTION('ref_axis',(-5.78241158658936E-16,-1.,-1.41228329145101E-48));
#4195=DIRECTION('',(5.78241158658936E-16,1.,1.77035296021731E-31));
#4196=DIRECTION('',(-1.22464679914735E-16,0.,1.));
#4197=DIRECTION('',(-5.78241158658936E-16,-1.,0.));
#4198=DIRECTION('',(1.22464679914735E-16,-7.08141184086923E-32,-1.));
#4199=DIRECTION('',(-5.78241158658936E-16,-1.,0.));
#4200=DIRECTION('',(-1.22464679914735E-16,0.,1.));
#4201=DIRECTION('',(-2.28847549044393E-17,-5.78241158658936E-16,1.));
#4202=DIRECTION('',(1.32329071915687E-32,-1.,-5.78241158658936E-16));
#4203=DIRECTION('',(-2.28847549044393E-17,-5.78241158658936E-16,1.));
#4204=DIRECTION('',(-1.22464679914735E-16,0.,1.));
#4205=DIRECTION('',(5.78241158658936E-16,1.,7.08141184086922E-32));
#4206=DIRECTION('',(1.22464679914735E-16,-1.09476442525376E-47,-1.));
#4207=DIRECTION('',(5.78241158658936E-16,1.,7.08141184086922E-32));
#4208=DIRECTION('center_axis',(-1.22464679914735E-16,0.,1.));
#4209=DIRECTION('ref_axis',(-1.,0.,-1.22464679914735E-16));
#4210=DIRECTION('',(-1.22464679914735E-16,0.,1.));
#4211=DIRECTION('center_axis',(0.,0.,-1.));
#4212=DIRECTION('ref_axis',(-1.,0.,0.));
#4213=DIRECTION('center_axis',(-1.,4.88654500275157E-16,-1.22464679914735E-16));
#4214=DIRECTION('ref_axis',(-4.88654500275157E-16,-1.,-3.23663765428249E-48));
#4215=DIRECTION('',(-1.22464679914735E-16,0.,1.));
#4216=DIRECTION('',(-2.28847549044393E-17,-5.78241158658936E-16,1.));
#4217=DIRECTION('',(1.32329071915687E-32,-1.,-5.78241158658936E-16));
#4218=DIRECTION('',(-2.28847549044393E-17,-5.78241158658936E-16,1.));
#4219=DIRECTION('',(-1.22464679914735E-16,0.,1.));
#4220=DIRECTION('',(4.88654500275157E-16,1.,1.4960729241273E-31));
#4221=DIRECTION('center_axis',(-1.22464679914735E-16,0.,1.));
#4222=DIRECTION('ref_axis',(-1.,0.,-1.22464679914735E-16));
#4223=DIRECTION('',(-1.22464679914735E-16,0.,1.));
#4224=DIRECTION('center_axis',(3.06161699786839E-16,0.,-1.));
#4225=DIRECTION('ref_axis',(-1.,0.,-3.06161699786839E-16));
#4226=DIRECTION('center_axis',(-4.88654500275157E-16,-1.,-5.9842916965092E-32));
#4227=DIRECTION('ref_axis',(1.,-4.88654500275157E-16,0.));
#4228=DIRECTION('',(-1.22464679914735E-16,0.,1.));
#4229=DIRECTION('',(1.,-4.88654500275157E-16,3.06161699786839E-16));
#4230=DIRECTION('center_axis',(-1.22464679914735E-16,0.,1.));
#4231=DIRECTION('ref_axis',(-1.,0.,-1.22464679914735E-16));
#4232=DIRECTION('',(-1.22464679914735E-16,0.,1.));
#4233=DIRECTION('center_axis',(3.06161699786839E-16,0.,-1.));
#4234=DIRECTION('ref_axis',(-1.,0.,-3.06161699786839E-16));
#4235=DIRECTION('center_axis',(1.,-4.88654500275157E-16,1.22464679914735E-16));
#4236=DIRECTION('ref_axis',(4.88654500275157E-16,1.,3.23663765428249E-48));
#4237=DIRECTION('',(-1.22464679914735E-16,0.,1.));
#4238=DIRECTION('',(-2.28847549044393E-17,-5.78241158658936E-16,1.));
#4239=DIRECTION('',(1.32329071915687E-32,-1.,-5.78241158658936E-16));
#4240=DIRECTION('',(-2.28847549044393E-17,-5.78241158658936E-16,1.));
#4241=DIRECTION('',(4.88654500275157E-16,1.,1.4960729241273E-31));
#4242=DIRECTION('center_axis',(-1.22464679914735E-16,0.,1.));
#4243=DIRECTION('ref_axis',(-1.,0.,-1.22464679914735E-16));
#4244=DIRECTION('',(-1.22464679914735E-16,0.,1.));
#4245=DIRECTION('center_axis',(3.06161699786839E-16,0.,-1.));
#4246=DIRECTION('ref_axis',(-1.,0.,-3.06161699786839E-16));
#4247=DIRECTION('center_axis',(0.,1.,0.));
#4248=DIRECTION('ref_axis',(0.,0.,-1.));
#4249=DIRECTION('',(-1.22464679914735E-16,0.,1.));
#4250=DIRECTION('',(1.,0.,3.06161699786839E-16));
#4251=DIRECTION('center_axis',(-1.22464679914735E-16,0.,1.));
#4252=DIRECTION('ref_axis',(-1.,0.,-1.22464679914735E-16));
#4253=DIRECTION('center_axis',(3.06161699786839E-16,0.,-1.));
#4254=DIRECTION('ref_axis',(-1.,0.,-3.06161699786839E-16));
#4255=DIRECTION('center_axis',(-3.06161699786839E-16,0.,1.));
#4256=DIRECTION('ref_axis',(1.,0.,3.06161699786839E-16));
#4257=DIRECTION('',(1.,-5.78241158658936E-16,3.06161699786839E-16));
#4258=DIRECTION('center_axis',(3.06161699786839E-16,0.,-1.));
#4259=DIRECTION('ref_axis',(-1.,0.,-3.06161699786839E-16));
#4260=DIRECTION('center_axis',(3.06161699786839E-16,0.,-1.));
#4261=DIRECTION('ref_axis',(-1.,0.,-3.06161699786839E-16));
#4262=DIRECTION('',(-5.78241158658936E-16,-1.,-1.77035296021731E-31));
#4263=DIRECTION('center_axis',(3.06161699786839E-16,0.,-1.));
#4264=DIRECTION('ref_axis',(-1.,0.,-3.06161699786839E-16));
#4265=DIRECTION('center_axis',(-1.22464679914735E-16,0.,1.));
#4266=DIRECTION('ref_axis',(-1.,0.,-1.22464679914735E-16));
#4267=DIRECTION('center_axis',(0.,0.,-1.));
#4268=DIRECTION('ref_axis',(-1.,0.,0.));
#4269=DIRECTION('',(-1.22464679914735E-16,0.,1.));
#4270=DIRECTION('center_axis',(5.78241158658936E-16,1.,7.08141184086922E-32));
#4271=DIRECTION('ref_axis',(-1.,5.78241158658936E-16,0.));
#4272=DIRECTION('',(-1.,5.78241158658936E-16,0.));
#4273=DIRECTION('',(-1.22464679914735E-16,0.,1.));
#4274=DIRECTION('',(-1.,5.78241158658936E-16,0.));
#4275=DIRECTION('',(0.,0.,1.));
#4276=DIRECTION('center_axis',(-1.22464679914735E-16,0.,1.));
#4277=DIRECTION('ref_axis',(-1.,0.,-1.22464679914735E-16));
#4278=DIRECTION('',(-1.22464679914735E-16,0.,1.));
#4279=DIRECTION('center_axis',(1.,-5.78241158658936E-16,1.22464679914735E-16));
#4280=DIRECTION('ref_axis',(5.78241158658936E-16,1.,1.41228329145101E-48));
#4281=DIRECTION('',(-1.22464679914735E-16,0.,1.));
#4282=DIRECTION('',(-2.28847549044393E-17,-5.78241158658936E-16,1.));
#4283=DIRECTION('',(1.32329071915687E-32,-1.,-5.78241158658936E-16));
#4284=DIRECTION('',(-2.28847549044393E-17,-5.78241158658936E-16,1.));
#4285=DIRECTION('center_axis',(-1.22464679914735E-16,0.,1.));
#4286=DIRECTION('ref_axis',(-1.,0.,-1.22464679914735E-16));
#4287=DIRECTION('center_axis',(-1.22464679914735E-16,0.,1.));
#4288=DIRECTION('ref_axis',(-1.,0.,-1.22464679914735E-16));
#4289=DIRECTION('center_axis',(0.,-7.08141184086922E-32,1.));
#4290=DIRECTION('ref_axis',(0.,-1.,-7.08141184086922E-32));
#4291=DIRECTION('center_axis',(0.,0.,1.));
#4292=DIRECTION('ref_axis',(-1.,0.,0.));
#4293=DIRECTION('',(5.78241158658936E-16,1.,0.));
#4294=DIRECTION('',(-1.,5.78241158658936E-16,0.));
#4295=DIRECTION('center_axis',(1.,-5.78241158658936E-16,0.));
#4296=DIRECTION('ref_axis',(5.78241158658936E-16,1.,0.));
#4297=DIRECTION('',(5.78241158658936E-16,1.,0.));
#4298=DIRECTION('',(0.,0.,1.));
#4299=DIRECTION('center_axis',(0.,0.,1.));
#4300=DIRECTION('ref_axis',(-1.,0.,0.));
#4301=DIRECTION('',(-1.,5.78241158658936E-16,0.));
#4302=DIRECTION('center_axis',(-5.78241158658936E-16,-1.,0.));
#4303=DIRECTION('ref_axis',(1.,-5.78241158658936E-16,0.));
#4304=DIRECTION('center_axis',(0.,7.08141184086922E-32,-1.));
#4305=DIRECTION('ref_axis',(0.,-1.,-7.08141184086922E-32));
#4306=DIRECTION('',(-1.,5.78241158658936E-16,4.09476378780532E-47));
#4307=DIRECTION('',(-5.78241158658936E-16,-1.,-7.08141184086922E-32));
#4308=DIRECTION('center_axis',(-1.,5.78241158658936E-16,0.));
#4309=DIRECTION('ref_axis',(-5.78241158658936E-16,-1.,0.));
#4310=DIRECTION('',(-4.09476378780532E-47,-7.08141184086922E-32,1.));
#4311=DIRECTION('',(-5.78241158658936E-16,-1.,-7.08141184086922E-32));
#4312=DIRECTION('center_axis',(0.,7.08141184086922E-32,-1.));
#4313=DIRECTION('ref_axis',(0.,-1.,-7.08141184086922E-32));
#4314=DIRECTION('',(-1.,5.78241158658936E-16,4.09476378780532E-47));
#4315=DIRECTION('center_axis',(-5.78241158658936E-16,-1.,-7.08141184086922E-32));
#4316=DIRECTION('ref_axis',(1.,-5.78241158658936E-16,-4.09476378780532E-47));
#4317=DIRECTION('center_axis',(1.78184314006146E-48,-1.,-5.78241158658936E-16));
#4318=DIRECTION('ref_axis',(-6.41902719210046E-80,-5.78241158658936E-16,
1.));
#4319=DIRECTION('',(-1.,1.32329071915687E-32,-2.28847549044393E-17));
#4320=DIRECTION('center_axis',(1.78184314006146E-48,-1.,-5.78241158658936E-16));
#4321=DIRECTION('ref_axis',(-6.41902719210046E-80,-5.78241158658936E-16,
1.));
#4322=DIRECTION('',(-1.,1.32329071915687E-32,-2.28847549044393E-17));
#4323=DIRECTION('center_axis',(-2.28847549044393E-17,-5.78241158658936E-16,
1.));
#4324=DIRECTION('ref_axis',(1.,-1.32329071915687E-32,2.28847549044393E-17));
#4325=DIRECTION('center_axis',(1.78184314006146E-48,-1.,-5.78241158658936E-16));
#4326=DIRECTION('ref_axis',(-6.41902719210046E-80,-5.78241158658936E-16,
1.));
#4327=DIRECTION('',(-1.,1.32329071915687E-32,-2.28847549044393E-17));
#4328=DIRECTION('center_axis',(1.78184314006146E-48,-1.,-5.78241158658936E-16));
#4329=DIRECTION('ref_axis',(-6.41902719210046E-80,-5.78241158658936E-16,
1.));
#4330=DIRECTION('',(-1.,1.32329071915687E-32,-2.28847549044393E-17));
#4331=DIRECTION('center_axis',(-2.28847549044393E-17,-5.78241158658936E-16,
1.));
#4332=DIRECTION('ref_axis',(1.,-1.32329071915687E-32,2.28847549044393E-17));
#4333=DIRECTION('axis',(0.,0.,1.));
#4334=DIRECTION('refdir',(1.,0.,0.));
#4335=DIRECTION('center_axis',(3.06161699786839E-16,-5.78241158658936E-16,
1.));
#4336=DIRECTION('ref_axis',(1.,1.77035296021731E-31,-3.06161699786839E-16));
#4337=DIRECTION('',(-1.77035296021731E-31,-1.,-5.78241158658936E-16));
#4338=DIRECTION('',(1.,1.77035296021731E-31,-3.06161699786839E-16));
#4339=DIRECTION('',(-1.77035296021731E-31,-1.,-5.78241158658936E-16));
#4340=DIRECTION('',(1.,1.77035296021731E-31,-3.06161699786839E-16));
#4341=DIRECTION('',(1.77035296021731E-31,1.,5.78241158658936E-16));
#4342=DIRECTION('',(1.,1.77035296021731E-31,-3.06161699786839E-16));
#4343=DIRECTION('',(1.77035296021731E-31,1.,5.78241158658936E-16));
#4344=DIRECTION('',(1.,1.77035296021731E-31,-3.06161699786839E-16));
#4345=DIRECTION('center_axis',(1.,-2.73691106313441E-47,-3.06161699786839E-16));
#4346=DIRECTION('ref_axis',(-3.06161699786839E-16,0.,-1.));
#4347=DIRECTION('',(-3.06161699786839E-16,5.78241158658936E-16,-1.));
#4348=DIRECTION('center_axis',(1.,-2.73691106313441E-47,-3.06161699786839E-16));
#4349=DIRECTION('ref_axis',(-3.06161699786839E-16,0.,-1.));
#4350=DIRECTION('',(-3.06161699786839E-16,5.78241158658936E-16,-1.));
#4351=DIRECTION('center_axis',(1.,-2.73691106313441E-47,-3.06161699786839E-16));
#4352=DIRECTION('ref_axis',(-3.06161699786839E-16,0.,-1.));
#4353=DIRECTION('center_axis',(1.,-2.73691106313441E-47,-3.06161699786839E-16));
#4354=DIRECTION('ref_axis',(-3.06161699786839E-16,0.,-1.));
#4355=DIRECTION('center_axis',(1.,-2.73691106313441E-47,-3.06161699786839E-16));
#4356=DIRECTION('ref_axis',(-3.06161699786839E-16,0.,-1.));
#4357=DIRECTION('',(-3.06161699786839E-16,5.78241158658936E-16,-1.));
#4358=DIRECTION('',(-3.06161699786839E-16,5.78241158658936E-16,-1.));
#4359=DIRECTION('center_axis',(1.,-2.73691106313441E-47,-3.06161699786839E-16));
#4360=DIRECTION('ref_axis',(-3.06161699786839E-16,0.,-1.));
#4361=DIRECTION('center_axis',(-1.,0.,3.06161699786839E-16));
#4362=DIRECTION('ref_axis',(3.06161699786839E-16,0.,1.));
#4363=DIRECTION('',(3.06161699786839E-16,-5.78241158658936E-16,1.));
#4364=DIRECTION('center_axis',(-1.,0.,3.06161699786839E-16));
#4365=DIRECTION('ref_axis',(3.06161699786839E-16,0.,1.));
#4366=DIRECTION('',(3.06161699786839E-16,-5.78241158658936E-16,1.));
#4367=DIRECTION('',(-1.77035296021731E-31,-1.,-5.78241158658936E-16));
#4368=DIRECTION('center_axis',(-1.,0.,3.06161699786839E-16));
#4369=DIRECTION('ref_axis',(3.06161699786839E-16,0.,1.));
#4370=DIRECTION('center_axis',(-1.,0.,3.06161699786839E-16));
#4371=DIRECTION('ref_axis',(3.06161699786839E-16,0.,1.));
#4372=DIRECTION('',(3.06161699786839E-16,-5.78241158658936E-16,1.));
#4373=DIRECTION('center_axis',(-1.,0.,3.06161699786839E-16));
#4374=DIRECTION('ref_axis',(3.06161699786839E-16,0.,1.));
#4375=DIRECTION('',(3.06161699786839E-16,-5.78241158658936E-16,1.));
#4376=DIRECTION('',(-1.77035296021731E-31,-1.,-5.78241158658936E-16));
#4377=DIRECTION('center_axis',(-1.,0.,3.06161699786839E-16));
#4378=DIRECTION('ref_axis',(3.06161699786839E-16,0.,1.));
#4379=DIRECTION('center_axis',(0.,1.,5.78241158658936E-16));
#4380=DIRECTION('ref_axis',(0.,-5.78241158658936E-16,1.));
#4381=DIRECTION('',(1.,-2.73691106313441E-47,-3.06161699786839E-16));
#4382=DIRECTION('',(1.,-2.73691106313441E-47,-3.06161699786839E-16));
#4383=DIRECTION('',(1.,1.77035296021731E-31,-3.06161699786839E-16));
#4384=DIRECTION('center_axis',(0.,1.,5.78241158658936E-16));
#4385=DIRECTION('ref_axis',(0.,-5.78241158658936E-16,1.));
#4386=DIRECTION('',(1.,-2.73691106313441E-47,-3.06161699786839E-16));
#4387=DIRECTION('',(1.,1.77035296021731E-31,-3.06161699786839E-16));
#4388=DIRECTION('',(1.,-2.73691106313441E-47,-3.06161699786839E-16));
#4389=DIRECTION('center_axis',(3.06161699786839E-16,-5.78241158658936E-16,
1.));
#4390=DIRECTION('ref_axis',(1.,1.77035296021731E-31,-3.06161699786839E-16));
#4391=DIRECTION('center_axis',(1.,-2.73691106313441E-47,-3.06161699786839E-16));
#4392=DIRECTION('ref_axis',(-3.06161699786839E-16,0.,-1.));
#4393=DIRECTION('',(1.,-2.73691106313441E-47,-3.06161699786839E-16));
#4394=DIRECTION('center_axis',(1.,-2.73691106313441E-47,-3.06161699786839E-16));
#4395=DIRECTION('ref_axis',(-3.06161699786839E-16,0.,-1.));
#4396=DIRECTION('',(1.,-2.73691106313441E-47,-3.06161699786839E-16));
#4397=DIRECTION('center_axis',(1.,-2.73691106313441E-47,-3.06161699786839E-16));
#4398=DIRECTION('ref_axis',(3.06161699786839E-16,1.22464679914735E-16,1.));
#4399=DIRECTION('center_axis',(1.,-2.73691106313441E-47,-3.06161699786839E-16));
#4400=DIRECTION('ref_axis',(3.06161699786839E-16,1.22464679914735E-16,1.));
#4401=DIRECTION('center_axis',(1.,-2.13821176807375E-47,-3.06161699786839E-16));
#4402=DIRECTION('ref_axis',(-3.06161699786839E-16,0.,-1.));
#4403=DIRECTION('',(3.06161699786839E-16,-5.78241158658936E-16,1.));
#4404=DIRECTION('',(1.77035296021731E-31,1.,5.78241158658936E-16));
#4405=DIRECTION('',(3.06161699786839E-16,-5.78241158658936E-16,1.));
#4406=DIRECTION('center_axis',(2.13821176807375E-47,-1.,-5.78241158658936E-16));
#4407=DIRECTION('ref_axis',(-7.75905768621749E-79,5.78241158658936E-16,
-1.));
#4408=DIRECTION('',(1.,1.77035296021731E-31,-3.06161699786839E-16));
#4409=DIRECTION('',(3.06161699786839E-16,-5.78241158658936E-16,1.));
#4410=DIRECTION('center_axis',(1.,-2.13821176807375E-47,-3.06161699786839E-16));
#4411=DIRECTION('ref_axis',(-3.06161699786839E-16,0.,-1.));
#4412=DIRECTION('',(1.77035296021731E-31,1.,5.78241158658936E-16));
#4413=DIRECTION('',(3.06161699786839E-16,-5.78241158658936E-16,1.));
#4414=DIRECTION('center_axis',(2.13821176807375E-47,-1.,-5.78241158658936E-16));
#4415=DIRECTION('ref_axis',(-7.75905768621749E-79,5.78241158658936E-16,
-1.));
#4416=DIRECTION('',(1.,1.77035296021731E-31,-3.06161699786839E-16));
#4417=DIRECTION('center_axis',(3.06161699786839E-16,-5.78241158658936E-16,
1.));
#4418=DIRECTION('ref_axis',(1.,1.77035296021731E-31,-3.06161699786839E-16));
#4419=DIRECTION('axis',(0.,0.,1.));
#4420=DIRECTION('refdir',(1.,0.,0.));
#4421=DIRECTION('center_axis',(1.77035296021731E-31,1.,5.78241158658936E-16));
#4422=DIRECTION('ref_axis',(-1.,1.77035296021731E-31,1.02369094695133E-46));
#4423=DIRECTION('',(-1.09476442525376E-47,5.78241158658936E-16,-1.));
#4424=DIRECTION('',(-1.,1.77035296021731E-31,0.));
#4425=DIRECTION('',(1.02369094695133E-46,5.78241158658936E-16,-1.));
#4426=DIRECTION('',(-1.,1.77035296021731E-31,0.));
#4427=DIRECTION('center_axis',(-1.,1.77035296021731E-31,0.));
#4428=DIRECTION('ref_axis',(-1.77035296021731E-31,-1.,0.));
#4429=DIRECTION('',(-1.77035296021731E-31,-1.,-5.78241158658936E-16));
#4430=DIRECTION('center_axis',(-1.,1.77035296021731E-31,0.));
#4431=DIRECTION('ref_axis',(-1.77035296021731E-31,-1.,0.));
#4432=DIRECTION('center_axis',(-1.,1.77035296021731E-31,0.));
#4433=DIRECTION('ref_axis',(-1.77035296021731E-31,-1.,0.));
#4434=DIRECTION('',(-1.77035296021731E-31,-1.,-5.78241158658936E-16));
#4435=DIRECTION('',(1.02369094695133E-46,5.78241158658936E-16,-1.));
#4436=DIRECTION('center_axis',(-1.,1.77035296021731E-31,0.));
#4437=DIRECTION('ref_axis',(-1.77035296021731E-31,-1.,0.));
#4438=DIRECTION('center_axis',(-1.,1.77035296021731E-31,0.));
#4439=DIRECTION('ref_axis',(-1.77035296021731E-31,-1.,0.));
#4440=DIRECTION('center_axis',(-1.,1.77035296021731E-31,0.));
#4441=DIRECTION('ref_axis',(-1.77035296021731E-31,-1.,0.));
#4442=DIRECTION('',(-1.77035296021731E-31,-1.,-5.78241158658936E-16));
#4443=DIRECTION('',(1.02369094695133E-46,5.78241158658936E-16,-1.));
#4444=DIRECTION('',(-1.77035296021731E-31,-1.,-5.78241158658936E-16));
#4445=DIRECTION('center_axis',(-1.,1.77035296021731E-31,0.));
#4446=DIRECTION('ref_axis',(-1.77035296021731E-31,-1.,0.));
#4447=DIRECTION('',(1.02369094695133E-46,5.78241158658936E-16,-1.));
#4448=DIRECTION('center_axis',(-1.,1.77035296021731E-31,0.));
#4449=DIRECTION('ref_axis',(-1.77035296021731E-31,-1.,0.));
#4450=DIRECTION('center_axis',(1.77035296021731E-31,1.,5.78241158658936E-16));
#4451=DIRECTION('ref_axis',(-1.,1.77035296021731E-31,1.02369094695133E-46));
#4452=DIRECTION('',(-1.,1.77035296021731E-31,0.));
#4453=DIRECTION('',(2.18952885050752E-47,5.78241158658936E-16,-1.));
#4454=DIRECTION('',(-1.,1.77035296021731E-31,0.));
#4455=DIRECTION('center_axis',(1.,1.34933644236765E-16,7.80241867855395E-32));
#4456=DIRECTION('ref_axis',(-1.34933644236765E-16,1.,3.27983892575899E-64));
#4457=DIRECTION('center_axis',(1.,1.34933644236765E-16,7.80241867855395E-32));
#4458=DIRECTION('ref_axis',(-1.34933644236765E-16,1.,3.27983892575899E-64));
#4459=DIRECTION('',(-1.34933644236765E-16,1.,5.78241158658936E-16));
#4460=DIRECTION('',(1.51929083932157E-62,-5.78241158658936E-16,1.));
#4461=DIRECTION('',(1.34933644236765E-16,-1.,-5.78241158658936E-16));
#4462=DIRECTION('center_axis',(1.,1.34933644236765E-16,7.80241867855395E-32));
#4463=DIRECTION('ref_axis',(-1.34933644236765E-16,1.,3.27983892575899E-64));
#4464=DIRECTION('center_axis',(1.,1.34933644236765E-16,7.80241867855395E-32));
#4465=DIRECTION('ref_axis',(-1.34933644236765E-16,1.,3.27983892575899E-64));
#4466=DIRECTION('center_axis',(1.,3.20467405062316E-16,1.85307443615657E-31));
#4467=DIRECTION('ref_axis',(-3.20467405062316E-16,1.,4.27650648726681E-63));
#4468=DIRECTION('center_axis',(1.,3.20467405062316E-16,1.85307443615657E-31));
#4469=DIRECTION('ref_axis',(-3.20467405062316E-16,1.,4.27650648726681E-63));
#4470=DIRECTION('center_axis',(1.,3.20467405062316E-16,1.85307443615657E-31));
#4471=DIRECTION('ref_axis',(-3.20467405062316E-16,1.,4.27650648726681E-63));
#4472=DIRECTION('',(3.20467405062316E-16,-1.,-5.78241158658936E-16));
#4473=DIRECTION('',(1.51929083932157E-62,-5.78241158658936E-16,1.));
#4474=DIRECTION('',(-3.20467405062316E-16,1.,5.78241158658936E-16));
#4475=DIRECTION('center_axis',(1.,3.20467405062316E-16,1.85307443615657E-31));
#4476=DIRECTION('ref_axis',(-3.20467405062316E-16,1.,4.27650648726681E-63));
#4477=DIRECTION('center_axis',(1.77035296021731E-31,1.,5.78241158658936E-16));
#4478=DIRECTION('ref_axis',(-1.,1.77035296021731E-31,1.02369094695133E-46));
#4479=DIRECTION('',(1.,-1.77035296021731E-31,-1.02369094695133E-46));
#4480=DIRECTION('',(1.,-1.77035296021731E-31,-1.02369094695133E-46));
#4481=DIRECTION('',(1.02369094695133E-46,5.78241158658936E-16,-1.));
#4482=DIRECTION('',(1.,-1.77035296021731E-31,-1.02369094695133E-46));
#4483=DIRECTION('',(1.02369094695133E-46,5.78241158658936E-16,-1.));
#4484=DIRECTION('',(1.,-1.77035296021731E-31,-1.02369094695133E-46));
#4485=DIRECTION('center_axis',(-1.51929083932157E-62,5.78241158658936E-16,
-1.));
#4486=DIRECTION('ref_axis',(0.,1.,5.78241158658936E-16));
#4487=DIRECTION('',(-1.,1.77035296021731E-31,0.));
#4488=DIRECTION('',(-1.,1.77035296021731E-31,0.));
#4489=DIRECTION('',(-1.,-8.7851649526921E-78,1.51929083932157E-62));
#4490=DIRECTION('center_axis',(-1.51929083932157E-62,5.78241158658936E-16,
-1.));
#4491=DIRECTION('ref_axis',(0.,1.,5.78241158658936E-16));
#4492=DIRECTION('',(-1.,1.77035296021731E-31,0.));
#4493=DIRECTION('',(1.,8.7851649526921E-78,-1.51929083932157E-62));
#4494=DIRECTION('',(-1.,1.77035296021731E-31,0.));
#4495=DIRECTION('center_axis',(-1.53655018820667E-93,-1.,-5.78241158658936E-16));
#4496=DIRECTION('ref_axis',(-4.01263672442025E-125,5.78241158658936E-16,
-1.));
#4497=DIRECTION('center_axis',(1.,-1.77035296021731E-31,0.));
#4498=DIRECTION('ref_axis',(1.77035296021731E-31,1.,0.));
#4499=DIRECTION('',(1.77035296021731E-31,1.,5.78241158658936E-16));
#4500=DIRECTION('',(1.02369094695133E-46,5.78241158658936E-16,-1.));
#4501=DIRECTION('',(1.77035296021731E-31,1.,5.78241158658936E-16));
#4502=DIRECTION('center_axis',(0.,-5.78241158658936E-16,1.));
#4503=DIRECTION('ref_axis',(0.,-1.,-5.78241158658936E-16));
#4504=DIRECTION('',(1.77035296021731E-31,1.,5.78241158658936E-16));
#4505=DIRECTION('',(1.,-1.77035296021731E-31,-1.02369094695133E-46));
#4506=DIRECTION('center_axis',(1.,-1.77035296021731E-31,0.));
#4507=DIRECTION('ref_axis',(1.77035296021731E-31,1.,0.));
#4508=DIRECTION('',(1.77035296021731E-31,1.,5.78241158658936E-16));
#4509=DIRECTION('',(1.02369094695133E-46,5.78241158658936E-16,-1.));
#4510=DIRECTION('center_axis',(0.,-5.78241158658936E-16,1.));
#4511=DIRECTION('ref_axis',(0.,-1.,-5.78241158658936E-16));
#4512=DIRECTION('',(1.,-1.77035296021731E-31,-1.02369094695133E-46));
#4513=DIRECTION('center_axis',(-1.77035296021731E-31,-1.,-5.78241158658936E-16));
#4514=DIRECTION('ref_axis',(1.,-1.77035296021731E-31,-1.02369094695133E-46));
#4515=DIRECTION('center_axis',(-1.,1.77035296021731E-31,0.));
#4516=DIRECTION('ref_axis',(-1.77035296021731E-31,-1.,0.));
#4517=DIRECTION('center_axis',(-1.,1.77035296021731E-31,0.));
#4518=DIRECTION('ref_axis',(-1.77035296021731E-31,-1.,0.));
#4519=DIRECTION('center_axis',(-1.,1.77035296021731E-31,0.));
#4520=DIRECTION('ref_axis',(-1.77035296021731E-31,-1.,0.));
#4521=DIRECTION('center_axis',(-1.,1.77035296021731E-31,0.));
#4522=DIRECTION('ref_axis',(-1.77035296021731E-31,-1.,0.));
#4523=DIRECTION('center_axis',(-1.,1.77035296021731E-31,0.));
#4524=DIRECTION('ref_axis',(-1.77035296021731E-31,-1.,0.));
#4525=DIRECTION('',(-1.,1.77035296021731E-31,0.));
#4526=DIRECTION('center_axis',(-1.,1.77035296021731E-31,0.));
#4527=DIRECTION('ref_axis',(-1.77035296021731E-31,-1.,0.));
#4528=DIRECTION('',(-1.,1.77035296021731E-31,0.));
#4529=DIRECTION('',(-0.0348905636596143,-1.21956388042974E-14,0.999391138927855));
#4530=DIRECTION('',(0.999391138927855,-1.24666961343951E-16,0.0348905636596143));
#4531=DIRECTION('',(-0.0348905636596143,-1.21956388042974E-14,0.999391138927855));
#4532=DIRECTION('',(0.999391138927855,-1.24666961343951E-16,0.0348905636596143));
#4533=DIRECTION('',(-0.0348905636596126,-1.23266230316106E-14,0.999391138927855));
#4534=DIRECTION('',(0.999391138927855,-4.16100505306033E-16,0.0348905636596126));
#4535=DIRECTION('',(0.0348905636596125,1.23266230316098E-14,-0.999391138927855));
#4536=DIRECTION('',(-0.999391138927855,4.16100505306032E-16,-0.0348905636596125));
#4537=DIRECTION('',(1.,3.44727761010536E-15,1.31318567131447E-15));
#4538=DIRECTION('',(1.31318567131448E-15,-3.86243623343318E-15,-1.));
#4539=DIRECTION('',(4.19476849887873E-15,-1.,-8.17940557192246E-15));
#4540=DIRECTION('',(0.999391138927855,3.90683039682812E-15,0.0348905636596166));
#4541=DIRECTION('',(-1.82353505700559E-15,2.82502949563069E-16,1.));
#4542=DIRECTION('',(1.,2.22044604925032E-16,1.82353505700559E-15));
#4543=DIRECTION('',(-1.53132714841855E-15,9.28566404293329E-15,-1.));
#4544=DIRECTION('',(-1.,-1.34614541735795E-15,1.53132714841854E-15));
#4545=DIRECTION('',(-0.0348905636596129,-1.21973284847381E-14,0.999391138927855));
#4546=DIRECTION('',(0.999391138927855,9.75097932898811E-17,0.0348905636596129));
#4547=DIRECTION('',(3.55965257270435E-15,-1.,-1.5986598413539E-14));
#4548=DIRECTION('',(1.,3.55965257270433E-15,1.31318567131445E-15));
#4549=CARTESIAN_POINT('',(0.,0.,0.));
#4550=CARTESIAN_POINT('',(0.,0.,0.));
#4551=CARTESIAN_POINT('Origin',(155.,858.5,147.));
#4552=CARTESIAN_POINT('',(151.,858.5,168.));
#4553=CARTESIAN_POINT('',(151.,858.5,172.));
#4554=CARTESIAN_POINT('',(151.,858.5,147.));
#4555=CARTESIAN_POINT('',(159.,858.5,168.));
#4556=CARTESIAN_POINT('',(360.,858.5,168.));
#4557=CARTESIAN_POINT('',(159.,858.5,172.));
#4558=CARTESIAN_POINT('',(159.,858.5,147.));
#4559=CARTESIAN_POINT('',(155.,858.5,172.));
#4560=CARTESIAN_POINT('Origin',(159.,850.,147.));
#4561=CARTESIAN_POINT('',(159.,841.5,168.));
#4562=CARTESIAN_POINT('',(159.,850.,168.));
#4563=CARTESIAN_POINT('',(159.,841.5,172.));
#4564=CARTESIAN_POINT('',(159.,841.5,147.));
#4565=CARTESIAN_POINT('',(159.,850.,172.));
#4566=CARTESIAN_POINT('Origin',(155.,841.5,147.));
#4567=CARTESIAN_POINT('',(151.,841.5,168.));
#4568=CARTESIAN_POINT('',(360.,841.5,168.));
#4569=CARTESIAN_POINT('',(151.,841.5,172.));
#4570=CARTESIAN_POINT('',(151.,841.5,147.));
#4571=CARTESIAN_POINT('',(155.,841.5,172.));
#4572=CARTESIAN_POINT('Origin',(151.,850.,147.));
#4573=CARTESIAN_POINT('',(151.,850.,168.));
#4574=CARTESIAN_POINT('',(151.,850.,172.));
#4575=CARTESIAN_POINT('Origin',(380.,850.,152.));
#4576=CARTESIAN_POINT('',(380.,830.,170.));
#4577=CARTESIAN_POINT('',(380.,830.,158.));
#4578=CARTESIAN_POINT('',(380.,830.,152.));
#4579=CARTESIAN_POINT('',(380.,834.,158.));
#4580=CARTESIAN_POINT('',(380.,850.,158.));
#4581=CARTESIAN_POINT('',(380.,834.,166.2));
#4582=CARTESIAN_POINT('',(380.,834.,152.));
#4583=CARTESIAN_POINT('',(380.,835.8,168.));
#4584=CARTESIAN_POINT('Origin',(380.,835.8,166.2));
#4585=CARTESIAN_POINT('',(380.,864.2,168.));
#4586=CARTESIAN_POINT('',(380.,850.,168.));
#4587=CARTESIAN_POINT('',(380.,866.,166.2));
#4588=CARTESIAN_POINT('Origin',(380.,864.2,166.2));
#4589=CARTESIAN_POINT('',(380.,866.,158.));
#4590=CARTESIAN_POINT('',(380.,866.,152.));
#4591=CARTESIAN_POINT('',(380.,870.,158.));
#4592=CARTESIAN_POINT('',(380.,850.,158.));
#4593=CARTESIAN_POINT('',(380.,870.,170.));
#4594=CARTESIAN_POINT('',(380.,870.,152.));
#4595=CARTESIAN_POINT('',(380.,868.,172.));
#4596=CARTESIAN_POINT('Origin',(380.,868.,170.));
#4597=CARTESIAN_POINT('',(380.,832.,172.));
#4598=CARTESIAN_POINT('',(380.,850.,172.));
#4599=CARTESIAN_POINT('Origin',(380.,832.,170.));
#4600=CARTESIAN_POINT('Origin',(-360.,866.,152.));
#4601=CARTESIAN_POINT('',(375.,866.,146.));
#4602=CARTESIAN_POINT('',(380.,866.,146.));
#4603=CARTESIAN_POINT('',(-360.,866.,146.));
#4604=CARTESIAN_POINT('',(375.,866.,158.));
#4605=CARTESIAN_POINT('',(375.,866.,152.));
#4606=CARTESIAN_POINT('',(-360.,866.,158.));
#4607=CARTESIAN_POINT('',(-380.,866.,166.2));
#4608=CARTESIAN_POINT('',(-360.,866.,166.2));
#4609=CARTESIAN_POINT('',(-380.,866.,158.));
#4610=CARTESIAN_POINT('',(-380.,866.,152.));
#4611=CARTESIAN_POINT('',(-375.,866.,158.));
#4612=CARTESIAN_POINT('',(-360.,866.,158.));
#4613=CARTESIAN_POINT('',(-375.,866.,146.));
#4614=CARTESIAN_POINT('',(-375.,866.,152.));
#4615=CARTESIAN_POINT('',(-380.,866.,146.));
#4616=CARTESIAN_POINT('',(-360.,866.,146.));
#4617=CARTESIAN_POINT('',(-380.,866.,137.8));
#4618=CARTESIAN_POINT('',(-380.,866.,152.));
#4619=CARTESIAN_POINT('',(380.,866.,137.8));
#4620=CARTESIAN_POINT('',(-360.,866.,137.8));
#4621=CARTESIAN_POINT('',(380.,866.,152.));
#4622=CARTESIAN_POINT('Origin',(-360.,834.,152.));
#4623=CARTESIAN_POINT('',(380.,834.,146.));
#4624=CARTESIAN_POINT('',(375.,834.,146.));
#4625=CARTESIAN_POINT('',(-360.,834.,146.));
#4626=CARTESIAN_POINT('',(380.,834.,137.8));
#4627=CARTESIAN_POINT('',(380.,834.,152.));
#4628=CARTESIAN_POINT('',(-380.,834.,137.8));
#4629=CARTESIAN_POINT('',(-360.,834.,137.8));
#4630=CARTESIAN_POINT('',(-380.,834.,146.));
#4631=CARTESIAN_POINT('',(-380.,834.,152.));
#4632=CARTESIAN_POINT('',(-375.,834.,146.));
#4633=CARTESIAN_POINT('',(-360.,834.,146.));
#4634=CARTESIAN_POINT('',(-375.,834.,158.));
#4635=CARTESIAN_POINT('',(-375.,834.,152.));
#4636=CARTESIAN_POINT('',(-380.,834.,158.));
#4637=CARTESIAN_POINT('',(-360.,834.,158.));
#4638=CARTESIAN_POINT('',(-380.,834.,166.2));
#4639=CARTESIAN_POINT('',(-380.,834.,152.));
#4640=CARTESIAN_POINT('',(-360.,834.,166.2));
#4641=CARTESIAN_POINT('',(375.,834.,158.));
#4642=CARTESIAN_POINT('',(-360.,834.,158.));
#4643=CARTESIAN_POINT('',(375.,834.,152.));
#4644=CARTESIAN_POINT('Origin',(-380.,850.,152.));
#4645=CARTESIAN_POINT('',(-380.,870.,146.));
#4646=CARTESIAN_POINT('',(-380.,850.,146.));
#4647=CARTESIAN_POINT('',(-380.,870.,134.));
#4648=CARTESIAN_POINT('',(-380.,870.,152.));
#4649=CARTESIAN_POINT('',(-380.,868.,132.));
#4650=CARTESIAN_POINT('Origin',(-380.,868.,134.));
#4651=CARTESIAN_POINT('',(-380.,832.,132.));
#4652=CARTESIAN_POINT('',(-380.,850.,132.));
#4653=CARTESIAN_POINT('',(-380.,830.,134.));
#4654=CARTESIAN_POINT('Origin',(-380.,832.,134.));
#4655=CARTESIAN_POINT('',(-380.,830.,146.));
#4656=CARTESIAN_POINT('',(-380.,830.,152.));
#4657=CARTESIAN_POINT('',(-380.,850.,146.));
#4658=CARTESIAN_POINT('',(-380.,835.8,136.));
#4659=CARTESIAN_POINT('Origin',(-380.,835.8,137.8));
#4660=CARTESIAN_POINT('',(-380.,864.2,136.));
#4661=CARTESIAN_POINT('',(-380.,850.,136.));
#4662=CARTESIAN_POINT('Origin',(-380.,864.2,137.8));
#4663=CARTESIAN_POINT('Origin',(-360.,870.,152.));
#4664=CARTESIAN_POINT('',(380.,870.,146.));
#4665=CARTESIAN_POINT('',(375.,870.,146.));
#4666=CARTESIAN_POINT('',(-360.,870.,146.));
#4667=CARTESIAN_POINT('',(380.,870.,134.));
#4668=CARTESIAN_POINT('',(380.,870.,152.));
#4669=CARTESIAN_POINT('',(-360.,870.,134.));
#4670=CARTESIAN_POINT('',(-375.,870.,146.));
#4671=CARTESIAN_POINT('',(-360.,870.,146.));
#4672=CARTESIAN_POINT('',(-375.,870.,158.));
#4673=CARTESIAN_POINT('',(-375.,870.,152.));
#4674=CARTESIAN_POINT('',(-380.,870.,158.));
#4675=CARTESIAN_POINT('',(-360.,870.,158.));
#4676=CARTESIAN_POINT('',(-380.,870.,170.));
#4677=CARTESIAN_POINT('',(-380.,870.,152.));
#4678=CARTESIAN_POINT('',(-360.,870.,170.));
#4679=CARTESIAN_POINT('',(375.,870.,158.));
#4680=CARTESIAN_POINT('',(-360.,870.,158.));
#4681=CARTESIAN_POINT('',(375.,870.,152.));
#4682=CARTESIAN_POINT('Origin',(-360.,830.,152.));
#4683=CARTESIAN_POINT('',(375.,830.,146.));
#4684=CARTESIAN_POINT('',(380.,830.,146.));
#4685=CARTESIAN_POINT('',(-360.,830.,146.));
#4686=CARTESIAN_POINT('',(375.,830.,158.));
#4687=CARTESIAN_POINT('',(375.,830.,152.));
#4688=CARTESIAN_POINT('',(-360.,830.,158.));
#4689=CARTESIAN_POINT('',(-380.,830.,170.));
#4690=CARTESIAN_POINT('',(-360.,830.,170.));
#4691=CARTESIAN_POINT('',(-380.,830.,158.));
#4692=CARTESIAN_POINT('',(-380.,830.,152.));
#4693=CARTESIAN_POINT('',(-375.,830.,158.));
#4694=CARTESIAN_POINT('',(-360.,830.,158.));
#4695=CARTESIAN_POINT('',(-375.,830.,146.));
#4696=CARTESIAN_POINT('',(-375.,830.,152.));
#4697=CARTESIAN_POINT('',(-360.,830.,146.));
#4698=CARTESIAN_POINT('',(380.,830.,134.));
#4699=CARTESIAN_POINT('',(-360.,830.,134.));
#4700=CARTESIAN_POINT('',(380.,830.,152.));
#4701=CARTESIAN_POINT('Origin',(-360.,850.,132.));
#4702=CARTESIAN_POINT('',(380.,832.,132.));
#4703=CARTESIAN_POINT('',(380.,868.,132.));
#4704=CARTESIAN_POINT('',(380.,850.,132.));
#4705=CARTESIAN_POINT('',(-360.,832.,132.));
#4706=CARTESIAN_POINT('',(-360.,868.,132.));
#4707=CARTESIAN_POINT('Origin',(-360.,832.,134.));
#4708=CARTESIAN_POINT('Origin',(380.,832.,134.));
#4709=CARTESIAN_POINT('Origin',(-360.,832.,170.));
#4710=CARTESIAN_POINT('',(-380.,832.,172.));
#4711=CARTESIAN_POINT('',(-360.,832.,172.));
#4712=CARTESIAN_POINT('Origin',(-380.,832.,170.));
#4713=CARTESIAN_POINT('Origin',(-360.,850.,172.));
#4714=CARTESIAN_POINT('',(-380.,868.,172.));
#4715=CARTESIAN_POINT('',(-360.,868.,172.));
#4716=CARTESIAN_POINT('',(-380.,850.,172.));
#4717=CARTESIAN_POINT('',(-159.,841.5,172.));
#4718=CARTESIAN_POINT('',(-151.,841.5,172.));
#4719=CARTESIAN_POINT('',(-155.,841.5,172.));
#4720=CARTESIAN_POINT('',(-159.,858.5,172.));
#4721=CARTESIAN_POINT('',(-159.,850.,172.));
#4722=CARTESIAN_POINT('',(-151.,858.5,172.));
#4723=CARTESIAN_POINT('',(-155.,858.5,172.));
#4724=CARTESIAN_POINT('',(-151.,850.,172.));
#4725=CARTESIAN_POINT('Origin',(-360.,868.,170.));
#4726=CARTESIAN_POINT('Origin',(-380.,868.,170.));
#4727=CARTESIAN_POINT('Origin',(-360.,868.,134.));
#4728=CARTESIAN_POINT('Origin',(380.,868.,134.));
#4729=CARTESIAN_POINT('Origin',(380.,850.,152.));
#4730=CARTESIAN_POINT('',(380.,850.,146.));
#4731=CARTESIAN_POINT('',(380.,850.,146.));
#4732=CARTESIAN_POINT('',(380.,864.2,136.));
#4733=CARTESIAN_POINT('Origin',(380.,864.2,137.8));
#4734=CARTESIAN_POINT('',(380.,835.8,136.));
#4735=CARTESIAN_POINT('',(380.,850.,136.));
#4736=CARTESIAN_POINT('Origin',(380.,835.8,137.8));
#4737=CARTESIAN_POINT('Origin',(-380.,850.,152.));
#4738=CARTESIAN_POINT('',(-380.,850.,158.));
#4739=CARTESIAN_POINT('',(-380.,864.2,168.));
#4740=CARTESIAN_POINT('Origin',(-380.,864.2,166.2));
#4741=CARTESIAN_POINT('',(-380.,835.8,168.));
#4742=CARTESIAN_POINT('',(-380.,850.,168.));
#4743=CARTESIAN_POINT('Origin',(-380.,835.8,166.2));
#4744=CARTESIAN_POINT('',(-380.,850.,158.));
#4745=CARTESIAN_POINT('Origin',(-360.,835.8,166.2));
#4746=CARTESIAN_POINT('',(-360.,835.8,168.));
#4747=CARTESIAN_POINT('Origin',(-360.,835.8,137.8));
#4748=CARTESIAN_POINT('',(-360.,835.8,136.));
#4749=CARTESIAN_POINT('Origin',(-360.,850.,136.));
#4750=CARTESIAN_POINT('',(-360.,864.2,136.));
#4751=CARTESIAN_POINT('Origin',(-360.,864.2,137.8));
#4752=CARTESIAN_POINT('Origin',(-360.,864.2,166.2));
#4753=CARTESIAN_POINT('',(-360.,864.2,168.));
#4754=CARTESIAN_POINT('Origin',(-360.,850.,168.));
#4755=CARTESIAN_POINT('',(-151.,841.5,168.));
#4756=CARTESIAN_POINT('',(-159.,841.5,168.));
#4757=CARTESIAN_POINT('',(-360.,841.5,168.));
#4758=CARTESIAN_POINT('',(-151.,858.5,168.));
#4759=CARTESIAN_POINT('',(-151.,850.,168.));
#4760=CARTESIAN_POINT('',(-159.,858.5,168.));
#4761=CARTESIAN_POINT('',(-360.,858.5,168.));
#4762=CARTESIAN_POINT('',(-159.,850.,168.));
#4763=CARTESIAN_POINT('Origin',(-378.,3982.26464896431,158.));
#4764=CARTESIAN_POINT('',(-375.,3982.26464896431,158.));
#4765=CARTESIAN_POINT('Origin',(-375.,3982.26464896431,152.));
#4766=CARTESIAN_POINT('',(-375.,3982.26464896431,146.));
#4767=CARTESIAN_POINT('Origin',(-378.,3982.26464896431,146.));
#4768=CARTESIAN_POINT('Origin',(-378.,3982.26464896431,146.));
#4769=CARTESIAN_POINT('',(-375.,3982.26464896431,146.));
#4770=CARTESIAN_POINT('Origin',(-375.,3982.26464896431,152.));
#4771=CARTESIAN_POINT('',(-375.,3982.26464896431,158.));
#4772=CARTESIAN_POINT('Origin',(-378.,3982.26464896431,158.));
#4773=CARTESIAN_POINT('Origin',(378.,3982.26464896431,146.));
#4774=CARTESIAN_POINT('',(375.,3982.26464896431,146.));
#4775=CARTESIAN_POINT('Origin',(378.,3982.26464896431,158.));
#4776=CARTESIAN_POINT('',(375.,3982.26464896431,158.));
#4777=CARTESIAN_POINT('Origin',(375.,3982.26464896431,152.));
#4778=CARTESIAN_POINT('Origin',(378.,3982.26464896431,146.));
#4779=CARTESIAN_POINT('',(375.,3982.26464896431,146.));
#4780=CARTESIAN_POINT('Origin',(378.,3982.26464896431,158.));
#4781=CARTESIAN_POINT('',(375.,3982.26464896431,158.));
#4782=CARTESIAN_POINT('Origin',(375.,3982.26464896431,152.));
#4783=CARTESIAN_POINT('Origin',(-155.,841.5,147.));
#4784=CARTESIAN_POINT('',(-159.,841.5,147.));
#4785=CARTESIAN_POINT('',(-151.,841.5,147.));
#4786=CARTESIAN_POINT('Origin',(-151.,850.,147.));
#4787=CARTESIAN_POINT('',(-151.,858.5,147.));
#4788=CARTESIAN_POINT('Origin',(-155.,858.5,147.));
#4789=CARTESIAN_POINT('',(-159.,858.5,147.));
#4790=CARTESIAN_POINT('Origin',(-159.,850.,147.));
#4791=CARTESIAN_POINT('',(0.,0.,0.));
#4792=CARTESIAN_POINT('Origin',(550.,850.,2188.));
#4793=CARTESIAN_POINT('',(550.,835.8,2188.));
#4794=CARTESIAN_POINT('',(-550.,835.8,2188.));
#4795=CARTESIAN_POINT('',(550.,835.8,2188.));
#4796=CARTESIAN_POINT('',(-550.,864.2,2188.));
#4797=CARTESIAN_POINT('',(-550.,850.,2188.));
#4798=CARTESIAN_POINT('',(550.,864.2,2188.));
#4799=CARTESIAN_POINT('',(550.,864.2,2188.));
#4800=CARTESIAN_POINT('',(550.,850.,2188.));
#4801=CARTESIAN_POINT('',(290.,840.,2188.));
#4802=CARTESIAN_POINT('',(280.,840.,2188.));
#4803=CARTESIAN_POINT('',(550.,840.,2188.));
#4804=CARTESIAN_POINT('',(290.,860.,2188.));
#4805=CARTESIAN_POINT('',(290.,850.,2188.));
#4806=CARTESIAN_POINT('',(280.,860.,2188.));
#4807=CARTESIAN_POINT('',(550.,860.,2188.));
#4808=CARTESIAN_POINT('',(280.,850.,2188.));
#4809=CARTESIAN_POINT('',(-290.,840.,2188.));
#4810=CARTESIAN_POINT('',(-280.,840.,2188.));
#4811=CARTESIAN_POINT('',(550.,840.,2188.));
#4812=CARTESIAN_POINT('',(-280.,860.,2188.));
#4813=CARTESIAN_POINT('',(-280.,850.,2188.));
#4814=CARTESIAN_POINT('',(-290.,860.,2188.));
#4815=CARTESIAN_POINT('',(550.,860.,2188.));
#4816=CARTESIAN_POINT('',(-290.,850.,2188.));
#4817=CARTESIAN_POINT('Origin',(550.,850.,2192.));
#4818=CARTESIAN_POINT('',(550.,868.,2192.));
#4819=CARTESIAN_POINT('',(-550.,868.,2192.));
#4820=CARTESIAN_POINT('',(550.,868.,2192.));
#4821=CARTESIAN_POINT('',(-550.,832.,2192.));
#4822=CARTESIAN_POINT('',(-550.,850.,2192.));
#4823=CARTESIAN_POINT('',(550.,832.,2192.));
#4824=CARTESIAN_POINT('',(550.,832.,2192.));
#4825=CARTESIAN_POINT('',(550.,850.,2192.));
#4826=CARTESIAN_POINT('',(280.,860.,2192.));
#4827=CARTESIAN_POINT('',(290.,860.,2192.));
#4828=CARTESIAN_POINT('',(285.,860.,2192.));
#4829=CARTESIAN_POINT('',(290.,840.,2192.));
#4830=CARTESIAN_POINT('',(290.,850.,2192.));
#4831=CARTESIAN_POINT('',(280.,840.,2192.));
#4832=CARTESIAN_POINT('',(285.,840.,2192.));
#4833=CARTESIAN_POINT('',(280.,850.,2192.));
#4834=CARTESIAN_POINT('',(-280.,860.,2192.));
#4835=CARTESIAN_POINT('',(-290.,860.,2192.));
#4836=CARTESIAN_POINT('',(-285.,860.,2192.));
#4837=CARTESIAN_POINT('',(-280.,840.,2192.));
#4838=CARTESIAN_POINT('',(-280.,850.,2192.));
#4839=CARTESIAN_POINT('',(-290.,840.,2192.));
#4840=CARTESIAN_POINT('',(-285.,840.,2192.));
#4841=CARTESIAN_POINT('',(-290.,850.,2192.));
#4842=CARTESIAN_POINT('Origin',(378.,856.,2177.));
#4843=CARTESIAN_POINT('',(381.,856.,2156.));
#4844=CARTESIAN_POINT('',(381.,856.,2152.));
#4845=CARTESIAN_POINT('',(381.,856.,2177.));
#4846=CARTESIAN_POINT('',(375.,856.,2156.));
#4847=CARTESIAN_POINT('',(-550.,856.,2156.));
#4848=CARTESIAN_POINT('',(375.,856.,2152.));
#4849=CARTESIAN_POINT('',(375.,856.,2177.));
#4850=CARTESIAN_POINT('',(378.,856.,2152.));
#4851=CARTESIAN_POINT('Origin',(375.,850.,2177.));
#4852=CARTESIAN_POINT('',(375.,844.,2156.));
#4853=CARTESIAN_POINT('',(375.,850.,2156.));
#4854=CARTESIAN_POINT('',(375.,844.,2152.));
#4855=CARTESIAN_POINT('',(375.,844.,2177.));
#4856=CARTESIAN_POINT('',(375.,850.,2152.));
#4857=CARTESIAN_POINT('Origin',(378.,844.,2177.));
#4858=CARTESIAN_POINT('',(381.,844.,2156.));
#4859=CARTESIAN_POINT('',(-550.,844.,2156.));
#4860=CARTESIAN_POINT('',(381.,844.,2152.));
#4861=CARTESIAN_POINT('',(381.,844.,2177.));
#4862=CARTESIAN_POINT('',(378.,844.,2152.));
#4863=CARTESIAN_POINT('Origin',(381.,850.,2177.));
#4864=CARTESIAN_POINT('',(381.,850.,2156.));
#4865=CARTESIAN_POINT('',(381.,850.,2152.));
#4866=CARTESIAN_POINT('Origin',(342.,856.,2177.));
#4867=CARTESIAN_POINT('',(345.,856.,2156.));
#4868=CARTESIAN_POINT('',(345.,856.,2152.));
#4869=CARTESIAN_POINT('',(345.,856.,2177.));
#4870=CARTESIAN_POINT('',(339.,856.,2156.));
#4871=CARTESIAN_POINT('',(-550.,856.,2156.));
#4872=CARTESIAN_POINT('',(339.,856.,2152.));
#4873=CARTESIAN_POINT('',(339.,856.,2177.));
#4874=CARTESIAN_POINT('',(342.,856.,2152.));
#4875=CARTESIAN_POINT('Origin',(339.,850.,2177.));
#4876=CARTESIAN_POINT('',(339.,844.,2156.));
#4877=CARTESIAN_POINT('',(339.,850.,2156.));
#4878=CARTESIAN_POINT('',(339.,844.,2152.));
#4879=CARTESIAN_POINT('',(339.,844.,2177.));
#4880=CARTESIAN_POINT('',(339.,850.,2152.));
#4881=CARTESIAN_POINT('Origin',(342.,844.,2177.));
#4882=CARTESIAN_POINT('',(345.,844.,2156.));
#4883=CARTESIAN_POINT('',(-550.,844.,2156.));
#4884=CARTESIAN_POINT('',(345.,844.,2152.));
#4885=CARTESIAN_POINT('',(345.,844.,2177.));
#4886=CARTESIAN_POINT('',(342.,844.,2152.));
#4887=CARTESIAN_POINT('Origin',(345.,850.,2177.));
#4888=CARTESIAN_POINT('',(345.,850.,2156.));
#4889=CARTESIAN_POINT('',(345.,850.,2152.));
#4890=CARTESIAN_POINT('Origin',(550.,850.,2156.));
#4891=CARTESIAN_POINT('',(550.,864.2,2156.));
#4892=CARTESIAN_POINT('',(-550.,864.2,2156.));
#4893=CARTESIAN_POINT('',(550.,864.2,2156.));
#4894=CARTESIAN_POINT('',(-550.,835.8,2156.));
#4895=CARTESIAN_POINT('',(-550.,850.,2156.));
#4896=CARTESIAN_POINT('',(550.,835.8,2156.));
#4897=CARTESIAN_POINT('',(550.,835.8,2156.));
#4898=CARTESIAN_POINT('',(550.,850.,2156.));
#4899=CARTESIAN_POINT('',(-375.,844.,2156.));
#4900=CARTESIAN_POINT('',(-381.,844.,2156.));
#4901=CARTESIAN_POINT('',(550.,844.,2156.));
#4902=CARTESIAN_POINT('',(-381.,856.,2156.));
#4903=CARTESIAN_POINT('',(-381.,850.,2156.));
#4904=CARTESIAN_POINT('',(-375.,856.,2156.));
#4905=CARTESIAN_POINT('',(550.,856.,2156.));
#4906=CARTESIAN_POINT('',(-375.,850.,2156.));
#4907=CARTESIAN_POINT('',(-345.,844.,2156.));
#4908=CARTESIAN_POINT('',(-339.,844.,2156.));
#4909=CARTESIAN_POINT('',(550.,844.,2156.));
#4910=CARTESIAN_POINT('',(-345.,856.,2156.));
#4911=CARTESIAN_POINT('',(-345.,850.,2156.));
#4912=CARTESIAN_POINT('',(-339.,856.,2156.));
#4913=CARTESIAN_POINT('',(550.,856.,2156.));
#4914=CARTESIAN_POINT('',(-339.,850.,2156.));
#4915=CARTESIAN_POINT('Origin',(550.,850.,2152.));
#4916=CARTESIAN_POINT('',(550.,832.,2152.));
#4917=CARTESIAN_POINT('',(-550.,832.,2152.));
#4918=CARTESIAN_POINT('',(550.,832.,2152.));
#4919=CARTESIAN_POINT('',(-550.,868.,2152.));
#4920=CARTESIAN_POINT('',(-550.,850.,2152.));
#4921=CARTESIAN_POINT('',(550.,868.,2152.));
#4922=CARTESIAN_POINT('',(550.,868.,2152.));
#4923=CARTESIAN_POINT('',(550.,850.,2152.));
#4924=CARTESIAN_POINT('',(-375.,856.,2152.));
#4925=CARTESIAN_POINT('',(-381.,856.,2152.));
#4926=CARTESIAN_POINT('',(-378.,856.,2152.));
#4927=CARTESIAN_POINT('',(-381.,844.,2152.));
#4928=CARTESIAN_POINT('',(-381.,850.,2152.));
#4929=CARTESIAN_POINT('',(-375.,844.,2152.));
#4930=CARTESIAN_POINT('',(-378.,844.,2152.));
#4931=CARTESIAN_POINT('',(-375.,850.,2152.));
#4932=CARTESIAN_POINT('',(-339.,856.,2152.));
#4933=CARTESIAN_POINT('',(-345.,856.,2152.));
#4934=CARTESIAN_POINT('',(-342.,856.,2152.));
#4935=CARTESIAN_POINT('',(-345.,844.,2152.));
#4936=CARTESIAN_POINT('',(-345.,850.,2152.));
#4937=CARTESIAN_POINT('',(-339.,844.,2152.));
#4938=CARTESIAN_POINT('',(-342.,844.,2152.));
#4939=CARTESIAN_POINT('',(-339.,850.,2152.));
#4940=CARTESIAN_POINT('Origin',(550.,830.,2172.));
#4941=CARTESIAN_POINT('',(-550.,830.,2154.));
#4942=CARTESIAN_POINT('',(-550.,830.,2190.));
#4943=CARTESIAN_POINT('',(-550.,830.,2172.));
#4944=CARTESIAN_POINT('',(550.,830.,2154.));
#4945=CARTESIAN_POINT('',(550.,830.,2154.));
#4946=CARTESIAN_POINT('',(550.,830.,2190.));
#4947=CARTESIAN_POINT('',(550.,830.,2172.));
#4948=CARTESIAN_POINT('',(550.,830.,2190.));
#4949=CARTESIAN_POINT('Origin',(550.,832.,2154.));
#4950=CARTESIAN_POINT('Origin',(-550.,832.,2154.));
#4951=CARTESIAN_POINT('Origin',(550.,832.,2154.));
#4952=CARTESIAN_POINT('Origin',(550.,868.,2154.));
#4953=CARTESIAN_POINT('',(-550.,870.,2154.));
#4954=CARTESIAN_POINT('Origin',(-550.,868.,2154.));
#4955=CARTESIAN_POINT('',(550.,870.,2154.));
#4956=CARTESIAN_POINT('',(550.,870.,2154.));
#4957=CARTESIAN_POINT('Origin',(550.,868.,2154.));
#4958=CARTESIAN_POINT('Origin',(550.,870.,2172.));
#4959=CARTESIAN_POINT('',(-550.,870.,2190.));
#4960=CARTESIAN_POINT('',(-550.,870.,2172.));
#4961=CARTESIAN_POINT('',(550.,870.,2190.));
#4962=CARTESIAN_POINT('',(550.,870.,2190.));
#4963=CARTESIAN_POINT('',(550.,870.,2172.));
#4964=CARTESIAN_POINT('Origin',(550.,868.,2190.));
#4965=CARTESIAN_POINT('Origin',(-550.,868.,2190.));
#4966=CARTESIAN_POINT('Origin',(550.,868.,2190.));
#4967=CARTESIAN_POINT('Origin',(550.,832.,2190.));
#4968=CARTESIAN_POINT('Origin',(-550.,832.,2190.));
#4969=CARTESIAN_POINT('Origin',(550.,832.,2190.));
#4970=CARTESIAN_POINT('Origin',(-550.,850.,2172.));
#4971=CARTESIAN_POINT('',(-550.,866.,2186.2));
#4972=CARTESIAN_POINT('Origin',(-550.,864.2,2186.2));
#4973=CARTESIAN_POINT('',(-550.,834.,2186.2));
#4974=CARTESIAN_POINT('Origin',(-550.,835.8,2186.2));
#4975=CARTESIAN_POINT('',(-550.,834.,2157.8));
#4976=CARTESIAN_POINT('',(-550.,834.,2172.));
#4977=CARTESIAN_POINT('Origin',(-550.,835.8,2157.8));
#4978=CARTESIAN_POINT('',(-550.,866.,2157.8));
#4979=CARTESIAN_POINT('Origin',(-550.,864.2,2157.8));
#4980=CARTESIAN_POINT('',(-550.,866.,2172.));
#4981=CARTESIAN_POINT('Origin',(550.,850.,2172.));
#4982=CARTESIAN_POINT('',(550.,866.,2186.2));
#4983=CARTESIAN_POINT('Origin',(550.,864.2,2186.2));
#4984=CARTESIAN_POINT('',(550.,866.,2157.8));
#4985=CARTESIAN_POINT('',(550.,866.,2172.));
#4986=CARTESIAN_POINT('Origin',(550.,864.2,2157.8));
#4987=CARTESIAN_POINT('',(550.,834.,2157.8));
#4988=CARTESIAN_POINT('Origin',(550.,835.8,2157.8));
#4989=CARTESIAN_POINT('',(550.,834.,2186.2));
#4990=CARTESIAN_POINT('',(550.,834.,2172.));
#4991=CARTESIAN_POINT('Origin',(550.,835.8,2186.2));
#4992=CARTESIAN_POINT('Origin',(550.,864.2,2157.8));
#4993=CARTESIAN_POINT('',(550.,866.,2157.8));
#4994=CARTESIAN_POINT('Origin',(550.,835.8,2157.8));
#4995=CARTESIAN_POINT('',(550.,834.,2157.8));
#4996=CARTESIAN_POINT('Origin',(550.,834.,2172.));
#4997=CARTESIAN_POINT('',(550.,834.,2186.2));
#4998=CARTESIAN_POINT('Origin',(550.,835.8,2186.2));
#4999=CARTESIAN_POINT('Origin',(550.,864.2,2186.2));
#5000=CARTESIAN_POINT('',(550.,866.,2186.2));
#5001=CARTESIAN_POINT('Origin',(550.,866.,2172.));
#5002=CARTESIAN_POINT('Origin',(-381.,850.,2177.));
#5003=CARTESIAN_POINT('',(-381.,844.,2177.));
#5004=CARTESIAN_POINT('',(-381.,856.,2177.));
#5005=CARTESIAN_POINT('Origin',(-378.,856.,2177.));
#5006=CARTESIAN_POINT('',(-375.,856.,2177.));
#5007=CARTESIAN_POINT('Origin',(-375.,850.,2177.));
#5008=CARTESIAN_POINT('',(-375.,844.,2177.));
#5009=CARTESIAN_POINT('Origin',(-378.,844.,2177.));
#5010=CARTESIAN_POINT('Origin',(-345.,850.,2177.));
#5011=CARTESIAN_POINT('',(-345.,844.,2177.));
#5012=CARTESIAN_POINT('',(-345.,856.,2177.));
#5013=CARTESIAN_POINT('Origin',(-342.,856.,2177.));
#5014=CARTESIAN_POINT('',(-339.,856.,2177.));
#5015=CARTESIAN_POINT('Origin',(-339.,850.,2177.));
#5016=CARTESIAN_POINT('',(-339.,844.,2177.));
#5017=CARTESIAN_POINT('Origin',(-342.,844.,2177.));
#5018=CARTESIAN_POINT('Origin',(290.,850.,2167.));
#5019=CARTESIAN_POINT('',(290.,840.,2167.));
#5020=CARTESIAN_POINT('',(290.,860.,2167.));
#5021=CARTESIAN_POINT('Origin',(285.,860.,2167.));
#5022=CARTESIAN_POINT('',(280.,860.,2167.));
#5023=CARTESIAN_POINT('Origin',(280.,850.,2167.));
#5024=CARTESIAN_POINT('',(280.,840.,2167.));
#5025=CARTESIAN_POINT('Origin',(285.,840.,2167.));
#5026=CARTESIAN_POINT('Origin',(-280.,850.,2167.));
#5027=CARTESIAN_POINT('',(-280.,840.,2167.));
#5028=CARTESIAN_POINT('',(-280.,860.,2167.));
#5029=CARTESIAN_POINT('Origin',(-285.,860.,2167.));
#5030=CARTESIAN_POINT('',(-290.,860.,2167.));
#5031=CARTESIAN_POINT('Origin',(-290.,850.,2167.));
#5032=CARTESIAN_POINT('',(-290.,840.,2167.));
#5033=CARTESIAN_POINT('Origin',(-285.,840.,2167.));
#5034=CARTESIAN_POINT('',(0.,0.,0.));
#5035=CARTESIAN_POINT('Origin',(375.,-72.5,0.));
#5036=CARTESIAN_POINT('',(380.,-72.5,11.5));
#5037=CARTESIAN_POINT('Origin',(375.,-72.5,11.5));
#5038=CARTESIAN_POINT('',(380.,-72.5,-11.5));
#5039=CARTESIAN_POINT('',(380.,-72.5,0.));
#5040=CARTESIAN_POINT('Origin',(375.,-72.5,-11.5));
#5041=CARTESIAN_POINT('Origin',(375.,-92.5,-11.5));
#5042=CARTESIAN_POINT('',(410.,-72.5,-11.5));
#5043=CARTESIAN_POINT('Origin',(375.,-72.5,-11.5));
#5044=CARTESIAN_POINT('Origin',(375.,-72.5,0.));
#5045=CARTESIAN_POINT('',(410.,-72.5,-5.));
#5046=CARTESIAN_POINT('',(410.,-72.5,0.));
#5047=CARTESIAN_POINT('Origin',(375.,-72.5,-5.));
#5048=CARTESIAN_POINT('Origin',(375.,-105.,-5.));
#5049=CARTESIAN_POINT('',(405.,-72.5,-5.));
#5050=CARTESIAN_POINT('Origin',(375.,-72.5,-5.));
#5051=CARTESIAN_POINT('Origin',(375.,-72.5,-9.65792954036421E-15));
#5052=CARTESIAN_POINT('',(405.,-72.5,5.));
#5053=CARTESIAN_POINT('Origin',(405.,-72.5,-9.65792954036421E-15));
#5054=CARTESIAN_POINT('Origin',(375.,-72.5,5.));
#5055=CARTESIAN_POINT('Origin',(375.,-105.,5.));
#5056=CARTESIAN_POINT('',(410.,-72.5,5.));
#5057=CARTESIAN_POINT('Origin',(375.,-72.5,5.));
#5058=CARTESIAN_POINT('Origin',(375.,-72.5,0.));
#5059=CARTESIAN_POINT('',(410.,-72.5,11.5));
#5060=CARTESIAN_POINT('',(410.,-72.5,0.));
#5061=CARTESIAN_POINT('Origin',(375.,-72.5,11.5));
#5062=CARTESIAN_POINT('Origin',(375.,-92.5,11.5));
#5063=CARTESIAN_POINT('',(0.,0.,0.));
#5064=CARTESIAN_POINT('Origin',(-442.474405060128,1574.77423490353,703.141071318876));
#5065=CARTESIAN_POINT('',(-442.474405060128,1574.77423490353,698.141071318876));
#5066=CARTESIAN_POINT('Origin',(-442.474405060128,1574.77423490353,703.141071318876));
#5067=CARTESIAN_POINT('Origin',(-472.474405060128,1574.77423490353,703.141071318876));
#5068=CARTESIAN_POINT('',(-502.474405060128,1574.77423490353,698.141071318876));
#5069=CARTESIAN_POINT('Origin',(-502.474405060128,1574.77423490353,703.141071318876));
#5070=CARTESIAN_POINT('',(-472.474405060128,1574.77423490353,698.141071318876));
#5071=CARTESIAN_POINT('Origin',(-502.474405060128,1574.77423490353,703.141071318876));
#5072=CARTESIAN_POINT('',(0.,0.,0.));
#5073=CARTESIAN_POINT('Origin',(-360.,850.,-2152.));
#5074=CARTESIAN_POINT('',(-340.,855.,-2152.));
#5075=CARTESIAN_POINT('',(-344.,855.,-2152.));
#5076=CARTESIAN_POINT('',(-342.,855.,-2152.));
#5077=CARTESIAN_POINT('',(-344.,864.2,-2152.));
#5078=CARTESIAN_POINT('',(-344.,850.,-2152.));
#5079=CARTESIAN_POINT('',(-345.8,866.,-2152.));
#5080=CARTESIAN_POINT('Origin',(-345.8,864.2,-2152.));
#5081=CARTESIAN_POINT('',(-374.2,866.,-2152.));
#5082=CARTESIAN_POINT('',(-360.,866.,-2152.));
#5083=CARTESIAN_POINT('',(-376.,864.2,-2152.));
#5084=CARTESIAN_POINT('Origin',(-374.2,864.2,-2152.));
#5085=CARTESIAN_POINT('',(-376.,855.,-2152.));
#5086=CARTESIAN_POINT('',(-376.,850.,-2152.));
#5087=CARTESIAN_POINT('',(-380.,855.,-2152.));
#5088=CARTESIAN_POINT('',(-378.,855.,-2152.));
#5089=CARTESIAN_POINT('',(-380.,868.,-2152.));
#5090=CARTESIAN_POINT('',(-380.,850.,-2152.));
#5091=CARTESIAN_POINT('',(-378.,870.,-2152.));
#5092=CARTESIAN_POINT('Origin',(-378.,868.,-2152.));
#5093=CARTESIAN_POINT('',(-342.,870.,-2152.));
#5094=CARTESIAN_POINT('',(-360.,870.,-2152.));
#5095=CARTESIAN_POINT('',(-340.,868.,-2152.));
#5096=CARTESIAN_POINT('Origin',(-342.,868.,-2152.));
#5097=CARTESIAN_POINT('',(-340.,850.,-2152.));
#5098=CARTESIAN_POINT('Origin',(-360.,850.,-2152.));
#5099=CARTESIAN_POINT('',(-340.,845.,-2152.));
#5100=CARTESIAN_POINT('',(-340.,832.,-2152.));
#5101=CARTESIAN_POINT('',(-340.,850.,-2152.));
#5102=CARTESIAN_POINT('',(-342.,830.,-2152.));
#5103=CARTESIAN_POINT('Origin',(-342.,832.,-2152.));
#5104=CARTESIAN_POINT('',(-378.,830.,-2152.));
#5105=CARTESIAN_POINT('',(-360.,830.,-2152.));
#5106=CARTESIAN_POINT('',(-380.,832.,-2152.));
#5107=CARTESIAN_POINT('Origin',(-378.,832.,-2152.));
#5108=CARTESIAN_POINT('',(-380.,845.,-2152.));
#5109=CARTESIAN_POINT('',(-380.,850.,-2152.));
#5110=CARTESIAN_POINT('',(-376.,845.,-2152.));
#5111=CARTESIAN_POINT('',(-378.,845.,-2152.));
#5112=CARTESIAN_POINT('',(-376.,835.8,-2152.));
#5113=CARTESIAN_POINT('',(-376.,850.,-2152.));
#5114=CARTESIAN_POINT('',(-374.2,834.,-2152.));
#5115=CARTESIAN_POINT('Origin',(-374.2,835.8,-2152.));
#5116=CARTESIAN_POINT('',(-345.8,834.,-2152.));
#5117=CARTESIAN_POINT('',(-360.,834.,-2152.));
#5118=CARTESIAN_POINT('',(-344.,835.8,-2152.));
#5119=CARTESIAN_POINT('Origin',(-345.8,835.8,-2152.));
#5120=CARTESIAN_POINT('',(-344.,845.,-2152.));
#5121=CARTESIAN_POINT('',(-344.,850.,-2152.));
#5122=CARTESIAN_POINT('',(-342.,845.,-2152.));
#5123=CARTESIAN_POINT('Origin',(-360.,830.,-2152.));
#5124=CARTESIAN_POINT('',(-375.,830.,-1958.));
#5125=CARTESIAN_POINT('',(-375.,830.,-1946.));
#5126=CARTESIAN_POINT('',(-375.,830.,-1952.));
#5127=CARTESIAN_POINT('',(-378.,830.,-1958.));
#5128=CARTESIAN_POINT('',(-378.,830.,-1958.));
#5129=CARTESIAN_POINT('',(-378.,830.,-2152.));
#5130=CARTESIAN_POINT('',(-342.,830.,-172.));
#5131=CARTESIAN_POINT('',(-342.,830.,-2152.));
#5132=CARTESIAN_POINT('',(-378.,830.,-172.));
#5133=CARTESIAN_POINT('',(-360.,830.,-172.));
#5134=CARTESIAN_POINT('',(-378.,830.,-1946.));
#5135=CARTESIAN_POINT('',(-378.,830.,-2152.));
#5136=CARTESIAN_POINT('',(-378.,830.,-1946.));
#5137=CARTESIAN_POINT('Origin',(-378.,832.,-2152.));
#5138=CARTESIAN_POINT('',(-380.,832.,-172.));
#5139=CARTESIAN_POINT('Origin',(-378.,832.,-172.));
#5140=CARTESIAN_POINT('',(-380.,832.,-1946.));
#5141=CARTESIAN_POINT('',(-380.,832.,-2152.));
#5142=CARTESIAN_POINT('Origin',(-378.,832.,-1946.));
#5143=CARTESIAN_POINT('Origin',(-380.,850.,-2152.));
#5144=CARTESIAN_POINT('',(-380.,868.,-172.));
#5145=CARTESIAN_POINT('',(-380.,850.,-172.));
#5146=CARTESIAN_POINT('',(-380.,868.,-1946.));
#5147=CARTESIAN_POINT('',(-380.,868.,-2152.));
#5148=CARTESIAN_POINT('',(-380.,867.,-1946.));
#5149=CARTESIAN_POINT('',(-380.,850.,-1946.));
#5150=CARTESIAN_POINT('',(-380.,867.,-1958.));
#5151=CARTESIAN_POINT('',(-380.,867.,-2152.));
#5152=CARTESIAN_POINT('',(-380.,868.,-1958.));
#5153=CARTESIAN_POINT('',(-380.,850.,-1958.));
#5154=CARTESIAN_POINT('',(-380.,868.,-2152.));
#5155=CARTESIAN_POINT('',(-380.,855.,-2155.));
#5156=CARTESIAN_POINT('',(-380.,855.,-2155.));
#5157=CARTESIAN_POINT('',(-380.,845.,-2155.));
#5158=CARTESIAN_POINT('',(-380.,850.,-2155.));
#5159=CARTESIAN_POINT('',(-380.,845.,-2155.));
#5160=CARTESIAN_POINT('',(-380.,832.,-1958.));
#5161=CARTESIAN_POINT('',(-380.,832.,-2152.));
#5162=CARTESIAN_POINT('',(-380.,834.,-1958.));
#5163=CARTESIAN_POINT('',(-380.,850.,-1958.));
#5164=CARTESIAN_POINT('',(-380.,834.,-1946.));
#5165=CARTESIAN_POINT('',(-380.,834.,-2152.));
#5166=CARTESIAN_POINT('',(-380.,850.,-1946.));
#5167=CARTESIAN_POINT('Origin',(-378.,868.,-2152.));
#5168=CARTESIAN_POINT('',(-378.,870.,-1958.));
#5169=CARTESIAN_POINT('',(-378.,870.,-2152.));
#5170=CARTESIAN_POINT('Origin',(-378.,868.,-1958.));
#5171=CARTESIAN_POINT('Origin',(-344.,850.,-2152.));
#5172=CARTESIAN_POINT('',(-344.,864.2,-172.));
#5173=CARTESIAN_POINT('',(-344.,864.2,-2152.));
#5174=CARTESIAN_POINT('',(-344.,855.,-2155.));
#5175=CARTESIAN_POINT('',(-344.,855.,-2155.));
#5176=CARTESIAN_POINT('',(-344.,845.,-2155.));
#5177=CARTESIAN_POINT('',(-344.,850.,-2155.));
#5178=CARTESIAN_POINT('',(-344.,845.,-2155.));
#5179=CARTESIAN_POINT('',(-344.,835.8,-172.));
#5180=CARTESIAN_POINT('',(-344.,835.8,-2152.));
#5181=CARTESIAN_POINT('',(-344.,850.,-172.));
#5182=CARTESIAN_POINT('Origin',(-345.8,864.2,-2152.));
#5183=CARTESIAN_POINT('',(-345.8,866.,-172.));
#5184=CARTESIAN_POINT('',(-345.8,866.,-2152.));
#5185=CARTESIAN_POINT('Origin',(-345.8,864.2,-172.));
#5186=CARTESIAN_POINT('Origin',(-360.,866.,-2152.));
#5187=CARTESIAN_POINT('',(-374.2,866.,-172.));
#5188=CARTESIAN_POINT('',(-374.2,866.,-2152.));
#5189=CARTESIAN_POINT('',(-360.,866.,-172.));
#5190=CARTESIAN_POINT('Origin',(-374.2,864.2,-2152.));
#5191=CARTESIAN_POINT('',(-376.,864.2,-172.));
#5192=CARTESIAN_POINT('',(-376.,864.2,-2152.));
#5193=CARTESIAN_POINT('Origin',(-374.2,864.2,-172.));
#5194=CARTESIAN_POINT('Origin',(-376.,850.,-2152.));
#5195=CARTESIAN_POINT('',(-376.,835.8,-172.));
#5196=CARTESIAN_POINT('',(-376.,835.8,-2152.));
#5197=CARTESIAN_POINT('',(-376.,845.,-2155.));
#5198=CARTESIAN_POINT('',(-376.,845.,-2155.));
#5199=CARTESIAN_POINT('',(-376.,855.,-2155.));
#5200=CARTESIAN_POINT('',(-376.,850.,-2155.));
#5201=CARTESIAN_POINT('',(-376.,855.,-2155.));
#5202=CARTESIAN_POINT('',(-376.,850.,-172.));
#5203=CARTESIAN_POINT('Origin',(-374.2,835.8,-2152.));
#5204=CARTESIAN_POINT('',(-374.2,834.,-172.));
#5205=CARTESIAN_POINT('',(-374.2,834.,-2152.));
#5206=CARTESIAN_POINT('Origin',(-374.2,835.8,-172.));
#5207=CARTESIAN_POINT('Origin',(-360.,834.,-2152.));
#5208=CARTESIAN_POINT('',(-345.8,834.,-172.));
#5209=CARTESIAN_POINT('',(-345.8,834.,-2152.));
#5210=CARTESIAN_POINT('',(-360.,834.,-172.));
#5211=CARTESIAN_POINT('Origin',(-345.8,835.8,-2152.));
#5212=CARTESIAN_POINT('Origin',(-345.8,835.8,-172.));
#5213=CARTESIAN_POINT('Origin',(-360.,850.,-172.));
#5214=CARTESIAN_POINT('',(-378.,870.,-172.));
#5215=CARTESIAN_POINT('',(-342.,870.,-172.));
#5216=CARTESIAN_POINT('',(-360.,870.,-172.));
#5217=CARTESIAN_POINT('Origin',(-378.,868.,-172.));
#5218=CARTESIAN_POINT('',(-340.,832.,-172.));
#5219=CARTESIAN_POINT('Origin',(-342.,832.,-172.));
#5220=CARTESIAN_POINT('',(-340.,868.,-172.));
#5221=CARTESIAN_POINT('',(-340.,850.,-172.));
#5222=CARTESIAN_POINT('Origin',(-342.,868.,-172.));
#5223=CARTESIAN_POINT('Origin',(-378.,868.,-2152.));
#5224=CARTESIAN_POINT('',(-378.,870.,-1946.));
#5225=CARTESIAN_POINT('Origin',(-378.,868.,-1946.));
#5226=CARTESIAN_POINT('',(-378.,870.,-2152.));
#5227=CARTESIAN_POINT('Origin',(-360.,870.,-2152.));
#5228=CARTESIAN_POINT('',(-375.,870.,-1946.));
#5229=CARTESIAN_POINT('',(-378.,870.,-1946.));
#5230=CARTESIAN_POINT('',(-342.,870.,-2152.));
#5231=CARTESIAN_POINT('',(-375.,870.,-1958.));
#5232=CARTESIAN_POINT('',(-378.,870.,-1958.));
#5233=CARTESIAN_POINT('',(-375.,870.,-1952.));
#5234=CARTESIAN_POINT('Origin',(-342.,868.,-2152.));
#5235=CARTESIAN_POINT('',(-340.,868.,-2152.));
#5236=CARTESIAN_POINT('Origin',(-340.,850.,-2152.));
#5237=CARTESIAN_POINT('',(-340.,832.,-2152.));
#5238=CARTESIAN_POINT('',(-340.,845.,-2155.));
#5239=CARTESIAN_POINT('',(-340.,845.,-2155.));
#5240=CARTESIAN_POINT('',(-340.,855.,-2155.));
#5241=CARTESIAN_POINT('',(-340.,850.,-2155.));
#5242=CARTESIAN_POINT('',(-340.,855.,-2155.));
#5243=CARTESIAN_POINT('Origin',(-342.,832.,-2152.));
#5244=CARTESIAN_POINT('Origin',(-378.,832.,-2152.));
#5245=CARTESIAN_POINT('Origin',(-378.,832.,-1958.));
#5246=CARTESIAN_POINT('Origin',(-378.,867.,-1946.));
#5247=CARTESIAN_POINT('',(-375.,867.,-1946.));
#5248=CARTESIAN_POINT('',(-375.,867.,-1946.));
#5249=CARTESIAN_POINT('',(-378.,867.,-1946.));
#5250=CARTESIAN_POINT('Origin',(-375.,867.,-1952.));
#5251=CARTESIAN_POINT('',(-375.,867.,-1958.));
#5252=CARTESIAN_POINT('',(-375.,867.,-1958.));
#5253=CARTESIAN_POINT('',(-375.,867.,-1952.));
#5254=CARTESIAN_POINT('Origin',(-378.,867.,-1958.));
#5255=CARTESIAN_POINT('',(-378.,867.,-1958.));
#5256=CARTESIAN_POINT('Origin',(-382.450381904372,867.,-1952.));
#5257=CARTESIAN_POINT('Origin',(-378.,834.,-1946.));
#5258=CARTESIAN_POINT('',(-375.,834.,-1946.));
#5259=CARTESIAN_POINT('',(-378.,834.,-1946.));
#5260=CARTESIAN_POINT('',(-375.,834.,-1946.));
#5261=CARTESIAN_POINT('Origin',(-375.,834.,-1952.));
#5262=CARTESIAN_POINT('',(-375.,834.,-1958.));
#5263=CARTESIAN_POINT('',(-375.,834.,-1952.));
#5264=CARTESIAN_POINT('',(-375.,834.,-1958.));
#5265=CARTESIAN_POINT('Origin',(-378.,834.,-1958.));
#5266=CARTESIAN_POINT('',(-378.,834.,-1958.));
#5267=CARTESIAN_POINT('Origin',(-382.450381904372,834.,-1952.));
#5268=CARTESIAN_POINT('Origin',(-378.,855.,-2155.));
#5269=CARTESIAN_POINT('',(-378.,855.,-2155.));
#5270=CARTESIAN_POINT('Origin',(-378.,845.,-2155.));
#5271=CARTESIAN_POINT('',(-378.,845.,-2155.));
#5272=CARTESIAN_POINT('Origin',(-360.,850.,-2155.));
#5273=CARTESIAN_POINT('Origin',(-342.,855.,-2155.));
#5274=CARTESIAN_POINT('',(-342.,855.,-2155.));
#5275=CARTESIAN_POINT('Origin',(-342.,845.,-2155.));
#5276=CARTESIAN_POINT('',(-342.,845.,-2155.));
#5277=CARTESIAN_POINT('Origin',(-360.,850.,-2155.));
#5278=CARTESIAN_POINT('',(0.,0.,0.));
#5279=CARTESIAN_POINT('Origin',(5.2659812363336E-14,876.65182352066,172.));
#5280=CARTESIAN_POINT('',(-150.,860.,172.));
#5281=CARTESIAN_POINT('',(-150.,840.,172.));
#5282=CARTESIAN_POINT('',(-150.,850.,172.));
#5283=CARTESIAN_POINT('',(-160.,840.,172.));
#5284=CARTESIAN_POINT('',(-155.,840.,172.));
#5285=CARTESIAN_POINT('',(-160.,860.,172.));
#5286=CARTESIAN_POINT('',(-160.,850.,172.));
#5287=CARTESIAN_POINT('',(-155.,860.,172.));
#5288=CARTESIAN_POINT('',(-158.,842.5,172.));
#5289=CARTESIAN_POINT('',(-158.,857.5,172.));
#5290=CARTESIAN_POINT('',(-158.,850.,172.));
#5291=CARTESIAN_POINT('',(-152.,842.5,172.));
#5292=CARTESIAN_POINT('',(-155.,842.5,172.));
#5293=CARTESIAN_POINT('',(-152.,857.5,172.));
#5294=CARTESIAN_POINT('',(-152.,850.,172.));
#5295=CARTESIAN_POINT('',(-155.,857.5,172.));
#5296=CARTESIAN_POINT('Origin',(-150.,850.,197.));
#5297=CARTESIAN_POINT('',(-150.,860.,187.));
#5298=CARTESIAN_POINT('',(-150.,860.,197.));
#5299=CARTESIAN_POINT('',(-150.,840.,187.));
#5300=CARTESIAN_POINT('Origin',(-150.,850.,187.));
#5301=CARTESIAN_POINT('',(-150.,840.,197.));
#5302=CARTESIAN_POINT('',(-150.,850.,190.999999999999));
#5303=CARTESIAN_POINT('Origin',(-150.,850.,187.));
#5304=CARTESIAN_POINT('Origin',(-160.,850.,197.));
#5305=CARTESIAN_POINT('',(-160.,860.,187.));
#5306=CARTESIAN_POINT('',(-160.,840.,187.));
#5307=CARTESIAN_POINT('Origin',(-160.,850.,187.));
#5308=CARTESIAN_POINT('',(-160.,860.,197.));
#5309=CARTESIAN_POINT('',(-160.,840.,197.));
#5310=CARTESIAN_POINT('',(-160.,850.,190.999999999999));
#5311=CARTESIAN_POINT('Origin',(-160.,850.,187.));
#5312=CARTESIAN_POINT('Origin',(-153.,850.,175.));
#5313=CARTESIAN_POINT('',(-153.,840.,175.));
#5314=CARTESIAN_POINT('',(-153.,840.,187.));
#5315=CARTESIAN_POINT('',(-153.,840.,197.));
#5316=CARTESIAN_POINT('',(-153.,860.,187.));
#5317=CARTESIAN_POINT('Origin',(-153.,850.,187.));
#5318=CARTESIAN_POINT('',(-153.,860.,175.));
#5319=CARTESIAN_POINT('',(-153.,860.,197.));
#5320=CARTESIAN_POINT('',(-153.,850.,175.));
#5321=CARTESIAN_POINT('',(-153.,850.,191.));
#5322=CARTESIAN_POINT('Origin',(-153.,850.,187.));
#5323=CARTESIAN_POINT('Origin',(-157.,850.,175.));
#5324=CARTESIAN_POINT('',(-157.,860.,175.));
#5325=CARTESIAN_POINT('',(-157.,860.,187.));
#5326=CARTESIAN_POINT('',(-157.,860.,197.));
#5327=CARTESIAN_POINT('',(-157.,840.,187.));
#5328=CARTESIAN_POINT('Origin',(-157.,850.,187.));
#5329=CARTESIAN_POINT('',(-157.,840.,175.));
#5330=CARTESIAN_POINT('',(-157.,840.,197.));
#5331=CARTESIAN_POINT('',(-157.,850.,175.));
#5332=CARTESIAN_POINT('',(-157.,850.,191.));
#5333=CARTESIAN_POINT('Origin',(-157.,850.,187.));
#5334=CARTESIAN_POINT('Origin',(-155.,860.,197.));
#5335=CARTESIAN_POINT('',(-3269.52807175403,860.,187.));
#5336=CARTESIAN_POINT('',(-3269.52807175403,860.,187.));
#5337=CARTESIAN_POINT('',(-155.,860.,175.));
#5338=CARTESIAN_POINT('Origin',(-155.,840.,197.));
#5339=CARTESIAN_POINT('',(-3269.52807175403,840.,187.));
#5340=CARTESIAN_POINT('',(-155.,840.,175.));
#5341=CARTESIAN_POINT('',(-3269.52807175403,840.,187.));
#5342=CARTESIAN_POINT('Origin',(-155.,850.,175.));
#5343=CARTESIAN_POINT('Origin',(-3269.52807175403,850.,187.));
#5344=CARTESIAN_POINT('',(-3269.52807175403,850.,191.));
#5345=CARTESIAN_POINT('Origin',(-3269.52807175403,850.,187.));
#5346=CARTESIAN_POINT('',(-3269.52807175403,850.,191.));
#5347=CARTESIAN_POINT('Origin',(-3269.52807175403,850.,187.));
#5348=CARTESIAN_POINT('Origin',(-3269.52807175403,850.,187.));
#5349=CARTESIAN_POINT('Origin',(-158.,850.,168.));
#5350=CARTESIAN_POINT('',(-158.,857.5,168.));
#5351=CARTESIAN_POINT('',(-158.,857.5,168.));
#5352=CARTESIAN_POINT('',(-158.,842.5,168.));
#5353=CARTESIAN_POINT('',(-158.,850.,168.));
#5354=CARTESIAN_POINT('',(-158.,842.5,168.));
#5355=CARTESIAN_POINT('Origin',(-155.,842.5,168.));
#5356=CARTESIAN_POINT('',(-152.,842.5,168.));
#5357=CARTESIAN_POINT('',(-155.,842.5,168.));
#5358=CARTESIAN_POINT('',(-152.,842.5,168.));
#5359=CARTESIAN_POINT('Origin',(-152.,850.,168.));
#5360=CARTESIAN_POINT('',(-152.,857.5,168.));
#5361=CARTESIAN_POINT('',(-152.,850.,168.));
#5362=CARTESIAN_POINT('',(-152.,857.5,168.));
#5363=CARTESIAN_POINT('Origin',(-155.,857.5,168.));
#5364=CARTESIAN_POINT('',(-155.,857.5,168.));
#5365=CARTESIAN_POINT('Origin',(-155.,850.,168.));
#5366=CARTESIAN_POINT('',(0.,0.,0.));
#5367=CARTESIAN_POINT('Origin',(-32.,950.,107.));
#5368=CARTESIAN_POINT('',(-51.499999999999,950.,110.));
#5369=CARTESIAN_POINT('',(-51.5,950.,104.));
#5370=CARTESIAN_POINT('',(-51.5,950.,107.));
#5371=CARTESIAN_POINT('',(-54.5,950.,104.));
#5372=CARTESIAN_POINT('',(3079.10575317586,950.,104.));
#5373=CARTESIAN_POINT('',(-54.5,950.,110.));
#5374=CARTESIAN_POINT('',(-54.5,950.,107.));
#5375=CARTESIAN_POINT('',(3079.10575317586,950.,110.));
#5376=CARTESIAN_POINT('Origin',(-54.5,950.,107.));
#5377=CARTESIAN_POINT('',(-54.5,935.,125.));
#5378=CARTESIAN_POINT('',(-54.5,870.,125.));
#5379=CARTESIAN_POINT('',(-54.5,950.,125.));
#5380=CARTESIAN_POINT('Origin',(-54.5,935.,110.));
#5381=CARTESIAN_POINT('',(-54.5,935.,89.));
#5382=CARTESIAN_POINT('Origin',(-54.5,935.,104.));
#5383=CARTESIAN_POINT('',(-54.5,870.,89.));
#5384=CARTESIAN_POINT('',(-54.5,950.,89.));
#5385=CARTESIAN_POINT('',(-54.5,870.,107.));
#5386=CARTESIAN_POINT('',(-54.4999999999999,925.,107.));
#5387=CARTESIAN_POINT('Origin',(-54.5,920.,107.));
#5388=CARTESIAN_POINT('Origin',(-9.5,950.,107.));
#5389=CARTESIAN_POINT('',(-9.49999999999918,935.,125.));
#5390=CARTESIAN_POINT('',(-9.4999999999974,950.,110.));
#5391=CARTESIAN_POINT('Origin',(-9.5,935.,110.));
#5392=CARTESIAN_POINT('',(-9.5,870.,125.));
#5393=CARTESIAN_POINT('',(-9.5,950.,125.));
#5394=CARTESIAN_POINT('',(-9.5,870.,89.));
#5395=CARTESIAN_POINT('',(-9.5,870.,107.));
#5396=CARTESIAN_POINT('',(-9.49999999999918,935.,89.));
#5397=CARTESIAN_POINT('',(-9.5,950.,89.));
#5398=CARTESIAN_POINT('',(-9.4999999999974,950.,104.));
#5399=CARTESIAN_POINT('Origin',(-9.5,935.,104.));
#5400=CARTESIAN_POINT('',(-9.5,950.,107.));
#5401=CARTESIAN_POINT('',(-9.49999999999989,925.,107.));
#5402=CARTESIAN_POINT('Origin',(-9.5,920.,107.));
#5403=CARTESIAN_POINT('Origin',(-32.,950.,107.));
#5404=CARTESIAN_POINT('',(-12.4999999999993,950.,104.));
#5405=CARTESIAN_POINT('',(3079.10575317586,950.,104.));
#5406=CARTESIAN_POINT('',(-12.5000000000002,950.,110.));
#5407=CARTESIAN_POINT('',(-12.5,950.,107.));
#5408=CARTESIAN_POINT('',(3079.10575317586,950.,110.));
#5409=CARTESIAN_POINT('Origin',(-51.5,924.424490483128,86.));
#5410=CARTESIAN_POINT('',(-51.5,935.,125.));
#5411=CARTESIAN_POINT('Origin',(-51.5,935.,110.));
#5412=CARTESIAN_POINT('',(-51.5,873.,125.));
#5413=CARTESIAN_POINT('',(-51.5,924.424490483128,125.));
#5414=CARTESIAN_POINT('',(-51.5,873.,89.));
#5415=CARTESIAN_POINT('',(-51.5,873.,86.));
#5416=CARTESIAN_POINT('',(-51.499999999999,935.,89.));
#5417=CARTESIAN_POINT('',(-51.5,950.,89.));
#5418=CARTESIAN_POINT('Origin',(-51.5,935.,104.));
#5419=CARTESIAN_POINT('',(-51.5,925.,107.));
#5420=CARTESIAN_POINT('Origin',(-51.5,920.,107.));
#5421=CARTESIAN_POINT('Origin',(-12.5,924.424490483128,86.));
#5422=CARTESIAN_POINT('',(-12.4999999999993,935.,125.));
#5423=CARTESIAN_POINT('Origin',(-12.5000000000002,935.,110.));
#5424=CARTESIAN_POINT('',(-12.5000000000002,935.,89.));
#5425=CARTESIAN_POINT('Origin',(-12.5000000000002,935.,104.));
#5426=CARTESIAN_POINT('',(-12.5,873.,89.));
#5427=CARTESIAN_POINT('',(-12.5,950.,89.));
#5428=CARTESIAN_POINT('',(-12.5,873.,125.));
#5429=CARTESIAN_POINT('',(-12.5,873.,86.));
#5430=CARTESIAN_POINT('',(-12.5,924.424490483128,125.));
#5431=CARTESIAN_POINT('',(-12.5000000000002,925.,107.));
#5432=CARTESIAN_POINT('Origin',(-12.5000000000002,920.,107.));
#5433=CARTESIAN_POINT('Origin',(-32.,870.,107.));
#5434=CARTESIAN_POINT('',(-32.,870.,89.));
#5435=CARTESIAN_POINT('',(-32.,870.,125.));
#5436=CARTESIAN_POINT('',(-36.,870.,116.));
#5437=CARTESIAN_POINT('',(-36.,870.,98.));
#5438=CARTESIAN_POINT('',(-36.,870.,107.));
#5439=CARTESIAN_POINT('',(-28.,870.,116.));
#5440=CARTESIAN_POINT('',(-32.,870.,116.));
#5441=CARTESIAN_POINT('',(-28.,870.,98.));
#5442=CARTESIAN_POINT('',(-28.,870.,107.));
#5443=CARTESIAN_POINT('',(-32.,870.,98.));
#5444=CARTESIAN_POINT('Origin',(-32.,950.,89.));
#5445=CARTESIAN_POINT('',(3079.10575317586,935.,89.));
#5446=CARTESIAN_POINT('',(3079.10575317586,935.,89.));
#5447=CARTESIAN_POINT('',(-32.,873.,89.));
#5448=CARTESIAN_POINT('Origin',(-32.,950.,125.));
#5449=CARTESIAN_POINT('',(3079.10575317586,935.,125.));
#5450=CARTESIAN_POINT('',(-32.,873.,125.));
#5451=CARTESIAN_POINT('',(3079.10575317586,935.,125.));
#5452=CARTESIAN_POINT('Origin',(-32.,873.,86.));
#5453=CARTESIAN_POINT('Origin',(-36.,866.,107.));
#5454=CARTESIAN_POINT('',(-36.,866.,98.));
#5455=CARTESIAN_POINT('',(-36.,866.,98.));
#5456=CARTESIAN_POINT('',(-36.,866.,116.));
#5457=CARTESIAN_POINT('',(-36.,866.,107.));
#5458=CARTESIAN_POINT('',(-36.,866.,116.));
#5459=CARTESIAN_POINT('Origin',(-32.,866.,98.));
#5460=CARTESIAN_POINT('',(-28.,866.,98.));
#5461=CARTESIAN_POINT('',(-28.,866.,98.));
#5462=CARTESIAN_POINT('',(-32.,866.,98.));
#5463=CARTESIAN_POINT('Origin',(-28.,866.,107.));
#5464=CARTESIAN_POINT('',(-28.,866.,116.));
#5465=CARTESIAN_POINT('',(-28.,866.,116.));
#5466=CARTESIAN_POINT('',(-28.,866.,107.));
#5467=CARTESIAN_POINT('Origin',(-32.,866.,116.));
#5468=CARTESIAN_POINT('',(-32.,866.,116.));
#5469=CARTESIAN_POINT('Origin',(-32.,866.,107.));
#5470=CARTESIAN_POINT('Origin',(3079.10575317586,935.,104.));
#5471=CARTESIAN_POINT('Origin',(3079.10575317586,935.,110.));
#5472=CARTESIAN_POINT('Origin',(3079.10575317586,935.,104.));
#5473=CARTESIAN_POINT('Origin',(3079.10575317586,935.,110.));
#5474=CARTESIAN_POINT('Origin',(3065.02807175404,920.,107.));
#5475=CARTESIAN_POINT('',(3065.02807175404,925.,107.));
#5476=CARTESIAN_POINT('Origin',(3065.02807175404,920.,107.));
#5477=CARTESIAN_POINT('',(3065.02807175404,925.,107.));
#5478=CARTESIAN_POINT('',(-86.6714680902416,726.794456602128,-1527.55767408176));
#5479=CARTESIAN_POINT('',(-86.6714680902416,726.794456602128,-1527.55767408176));
#5480=CARTESIAN_POINT('',(-87.6708592291751,726.794456602126,-1527.59256464541));
#5481=CARTESIAN_POINT('',(-806.2330881183,726.794456602127,-1552.67887991668));
#5482=CARTESIAN_POINT('',(-451.119101094897,1647.29445660211,1077.95454842317));
#5483=CARTESIAN_POINT('',(184.01019779187,1681.79445660211,-195.302279739017));
#5484=CARTESIAN_POINT('',(21.8687159942891,0.0202216985744055,-0.186522895697117));
#5485=CARTESIAN_POINT('',(-163.961756128128,726.794456602129,-1517.07493259204));
#5486=CARTESIAN_POINT('',(222.140393838469,725.794456602128,-1516.77648991094));
#5487=CARTESIAN_POINT('',(-417.974405060132,1681.79445660212,-217.045451576823));
#5488=UNCERTAINTY_MEASURE_WITH_UNIT(LENGTH_MEASURE(0.01),#5506,
'DISTANCE_ACCURACY_VALUE',
'Maximum model space distance between geometric entities at asserted c
onnectivities');
#5489=UNCERTAINTY_MEASURE_WITH_UNIT(LENGTH_MEASURE(0.01),#5506,
'DISTANCE_ACCURACY_VALUE',
'Maximum model space distance between geometric entities at asserted c
onnectivities');
#5490=UNCERTAINTY_MEASURE_WITH_UNIT(LENGTH_MEASURE(0.01),#5506,
'DISTANCE_ACCURACY_VALUE',
'Maximum model space distance between geometric entities at asserted c
onnectivities');
#5491=UNCERTAINTY_MEASURE_WITH_UNIT(LENGTH_MEASURE(0.01),#5506,
'DISTANCE_ACCURACY_VALUE',
'Maximum model space distance between geometric entities at asserted c
onnectivities');
#5492=UNCERTAINTY_MEASURE_WITH_UNIT(LENGTH_MEASURE(0.01),#5506,
'DISTANCE_ACCURACY_VALUE',
'Maximum model space distance between geometric entities at asserted c
onnectivities');
#5493=UNCERTAINTY_MEASURE_WITH_UNIT(LENGTH_MEASURE(0.01),#5506,
'DISTANCE_ACCURACY_VALUE',
'Maximum model space distance between geometric entities at asserted c
onnectivities');
#5494=UNCERTAINTY_MEASURE_WITH_UNIT(LENGTH_MEASURE(0.01),#5506,
'DISTANCE_ACCURACY_VALUE',
'Maximum model space distance between geometric entities at asserted c
onnectivities');
#5495=UNCERTAINTY_MEASURE_WITH_UNIT(LENGTH_MEASURE(0.01),#5506,
'DISTANCE_ACCURACY_VALUE',
'Maximum model space distance between geometric entities at asserted c
onnectivities');
#5496=UNCERTAINTY_MEASURE_WITH_UNIT(LENGTH_MEASURE(0.01),#5506,
'DISTANCE_ACCURACY_VALUE',
'Maximum model space distance between geometric entities at asserted c
onnectivities');
#5497=(
GEOMETRIC_REPRESENTATION_CONTEXT(3)
GLOBAL_UNCERTAINTY_ASSIGNED_CONTEXT((#5488))
GLOBAL_UNIT_ASSIGNED_CONTEXT((#5506,#5508,#5509))
REPRESENTATION_CONTEXT('','3D')
);
#5498=(
GEOMETRIC_REPRESENTATION_CONTEXT(3)
GLOBAL_UNCERTAINTY_ASSIGNED_CONTEXT((#5489))
GLOBAL_UNIT_ASSIGNED_CONTEXT((#5506,#5508,#5509))
REPRESENTATION_CONTEXT('','3D')
);
#5499=(
GEOMETRIC_REPRESENTATION_CONTEXT(3)
GLOBAL_UNCERTAINTY_ASSIGNED_CONTEXT((#5490))
GLOBAL_UNIT_ASSIGNED_CONTEXT((#5506,#5508,#5509))
REPRESENTATION_CONTEXT('','3D')
);
#5500=(
GEOMETRIC_REPRESENTATION_CONTEXT(3)
GLOBAL_UNCERTAINTY_ASSIGNED_CONTEXT((#5491))
GLOBAL_UNIT_ASSIGNED_CONTEXT((#5506,#5508,#5509))
REPRESENTATION_CONTEXT('','3D')
);
#5501=(
GEOMETRIC_REPRESENTATION_CONTEXT(3)
GLOBAL_UNCERTAINTY_ASSIGNED_CONTEXT((#5492))
GLOBAL_UNIT_ASSIGNED_CONTEXT((#5506,#5508,#5509))
REPRESENTATION_CONTEXT('','3D')
);
#5502=(
GEOMETRIC_REPRESENTATION_CONTEXT(3)
GLOBAL_UNCERTAINTY_ASSIGNED_CONTEXT((#5493))
GLOBAL_UNIT_ASSIGNED_CONTEXT((#5506,#5508,#5509))
REPRESENTATION_CONTEXT('','3D')
);
#5503=(
GEOMETRIC_REPRESENTATION_CONTEXT(3)
GLOBAL_UNCERTAINTY_ASSIGNED_CONTEXT((#5494))
GLOBAL_UNIT_ASSIGNED_CONTEXT((#5506,#5508,#5509))
REPRESENTATION_CONTEXT('','3D')
);
#5504=(
GEOMETRIC_REPRESENTATION_CONTEXT(3)
GLOBAL_UNCERTAINTY_ASSIGNED_CONTEXT((#5495))
GLOBAL_UNIT_ASSIGNED_CONTEXT((#5506,#5508,#5509))
REPRESENTATION_CONTEXT('','3D')
);
#5505=(
GEOMETRIC_REPRESENTATION_CONTEXT(3)
GLOBAL_UNCERTAINTY_ASSIGNED_CONTEXT((#5496))
GLOBAL_UNIT_ASSIGNED_CONTEXT((#5506,#5508,#5509))
REPRESENTATION_CONTEXT('','3D')
);
#5506=(
LENGTH_UNIT()
NAMED_UNIT(*)
SI_UNIT(.MILLI.,.METRE.)
);
#5507=(
LENGTH_UNIT()
NAMED_UNIT(*)
SI_UNIT($,.METRE.)
);
#5508=(
NAMED_UNIT(*)
PLANE_ANGLE_UNIT()
SI_UNIT($,.RADIAN.)
);
#5509=(
NAMED_UNIT(*)
SI_UNIT($,.STERADIAN.)
SOLID_ANGLE_UNIT()
);
#5510=SHAPE_DEFINITION_REPRESENTATION(#5518,#5536);
#5511=SHAPE_DEFINITION_REPRESENTATION(#5519,#5537);
#5512=SHAPE_DEFINITION_REPRESENTATION(#5520,#5538);
#5513=SHAPE_DEFINITION_REPRESENTATION(#5521,#5539);
#5514=SHAPE_DEFINITION_REPRESENTATION(#5522,#5540);
#5515=SHAPE_DEFINITION_REPRESENTATION(#5523,#5541);
#5516=SHAPE_DEFINITION_REPRESENTATION(#5524,#5542);
#5517=SHAPE_DEFINITION_REPRESENTATION(#5525,#5543);
#5518=PRODUCT_DEFINITION_SHAPE('',$,#5545);
#5519=PRODUCT_DEFINITION_SHAPE('',$,#5546);
#5520=PRODUCT_DEFINITION_SHAPE('',$,#5547);
#5521=PRODUCT_DEFINITION_SHAPE('',$,#5548);
#5522=PRODUCT_DEFINITION_SHAPE('',$,#5549);
#5523=PRODUCT_DEFINITION_SHAPE('',$,#5550);
#5524=PRODUCT_DEFINITION_SHAPE('',$,#5551);
#5525=PRODUCT_DEFINITION_SHAPE('',$,#5552);
#5526=PRODUCT_DEFINITION_SHAPE($,$,#41);
#5527=PRODUCT_DEFINITION_SHAPE($,$,#42);
#5528=PRODUCT_DEFINITION_SHAPE($,$,#43);
#5529=PRODUCT_DEFINITION_SHAPE($,$,#44);
#5530=PRODUCT_DEFINITION_SHAPE($,$,#45);
#5531=PRODUCT_DEFINITION_SHAPE($,$,#46);
#5532=PRODUCT_DEFINITION_SHAPE($,$,#47);
#5533=PRODUCT_DEFINITION_SHAPE($,$,#48);
#5534=PRODUCT_DEFINITION_SHAPE($,$,#49);
#5535=PRODUCT_DEFINITION_SHAPE($,$,#50);
#5536=SHAPE_REPRESENTATION('',(#3378,#3635,#3636,#3637,#3638,#3639,#3640,
#3641,#3642,#3643,#3644),#5497);
#5537=SHAPE_REPRESENTATION('',(#3379),#5498);
#5538=SHAPE_REPRESENTATION('',(#3436),#5499);
#5539=SHAPE_REPRESENTATION('',(#3495),#5500);
#5540=SHAPE_REPRESENTATION('',(#3513),#5501);
#5541=SHAPE_REPRESENTATION('',(#3519),#5502);
#5542=SHAPE_REPRESENTATION('',(#3575),#5503);
#5543=SHAPE_REPRESENTATION('',(#3601),#5504);
#5544=PRODUCT_DEFINITION_CONTEXT('part definition',#5570,'design');
#5545=PRODUCT_DEFINITION('2026-10-07-09-57-01-875','MAS-605',
#5553,#5544);
#5546=PRODUCT_DEFINITION('Mast-bottom','Mast-bottom',#5554,#5544);
#5547=PRODUCT_DEFINITION('Mast-top-hinge','Mast-top-hinge',#5555,#5544);
#5548=PRODUCT_DEFINITION('2026-10-07-17-01-32-968','Pulley',#5556,#5544);
#5549=PRODUCT_DEFINITION('2026-10-07-10-38-52-522','rod',#5557,#5544);
#5550=PRODUCT_DEFINITION('Mast-third-vert-Mirrored',
'Mast-third-vert-Mirrored',#5558,#5544);
#5551=PRODUCT_DEFINITION('Mast_bottom_hook','Mast_bottom_hook',#5559,#5544);
#5552=PRODUCT_DEFINITION('2026-10-07-17-03-48-181','Part 103',#5560,#5544);
#5553=PRODUCT_DEFINITION_FORMATION('',$,#5572);
#5554=PRODUCT_DEFINITION_FORMATION('',$,#5573);
#5555=PRODUCT_DEFINITION_FORMATION('',$,#5574);
#5556=PRODUCT_DEFINITION_FORMATION('',$,#5575);
#5557=PRODUCT_DEFINITION_FORMATION('',$,#5576);
#5558=PRODUCT_DEFINITION_FORMATION('',$,#5577);
#5559=PRODUCT_DEFINITION_FORMATION('',$,#5578);
#5560=PRODUCT_DEFINITION_FORMATION('',$,#5579);
#5561=PRODUCT_RELATED_PRODUCT_CATEGORY('MAS-605',
'MAS-605',(#5572));
#5562=PRODUCT_RELATED_PRODUCT_CATEGORY('Mast-bottom','Mast-bottom',(#5573));
#5563=PRODUCT_RELATED_PRODUCT_CATEGORY('Mast-top-hinge',
'Mast-top-hinge',(#5574));
#5564=PRODUCT_RELATED_PRODUCT_CATEGORY('Pulley','Pulley',(#5575));
#5565=PRODUCT_RELATED_PRODUCT_CATEGORY('rod','rod',(#5576));
#5566=PRODUCT_RELATED_PRODUCT_CATEGORY('Mast-third-vert-Mirrored',
'Mast-third-vert-Mirrored',(#5577));
#5567=PRODUCT_RELATED_PRODUCT_CATEGORY('Mast_bottom_hook',
'Mast_bottom_hook',(#5578));
#5568=PRODUCT_RELATED_PRODUCT_CATEGORY('Part 103','Part 103',(#5579));
#5569=APPLICATION_PROTOCOL_DEFINITION('international standard',
'automotive_design',2009,#5570);
#5570=APPLICATION_CONTEXT(
'Core Data for Automotive Mechanical Design Process');
#5571=PRODUCT_CONTEXT('part definition',#5570,'mechanical');
#5572=PRODUCT('2026-10-07-09-57-01-875','MAS-605',$,(#5571));
#5573=PRODUCT('Mast-bottom','Mast-bottom','40x40x3mm-2pcs-mast-bottom',
(#5571));
#5574=PRODUCT('Mast-top-hinge','Mast-top-hinge',
'40x40x3mm-2pcs-third-mast-top-hinge',(#5571));
#5575=PRODUCT('2026-10-07-17-01-32-968','Pulley','20pcs-pulley',(#5571));
#5576=PRODUCT('2026-10-07-10-38-52-522','rod',$,(#5571));
#5577=PRODUCT('Mast-third-vert-Mirrored','Mast-third-vert-Mirrored',
'40x40x3mm-4pcs-mast-third-vert-Mirrored',(#5571));
#5578=PRODUCT('Mast_bottom_hook','Mast_bottom_hook',
'3mm_8pcs_second_mast_bottom_hook',(#5571));
#5579=PRODUCT('2026-10-07-17-03-48-181','Part 103','Part 103',(#5571));
#5580=PRESENTATION_STYLE_ASSIGNMENT((#5588));
#5581=PRESENTATION_STYLE_ASSIGNMENT((#5589));
#5582=PRESENTATION_STYLE_ASSIGNMENT((#5590));
#5583=PRESENTATION_STYLE_ASSIGNMENT((#5591));
#5584=PRESENTATION_STYLE_ASSIGNMENT((#5592));
#5585=PRESENTATION_STYLE_ASSIGNMENT((#5593));
#5586=PRESENTATION_STYLE_ASSIGNMENT((#5594));
#5587=PRESENTATION_STYLE_ASSIGNMENT((#5595));
#5588=SURFACE_STYLE_USAGE(.BOTH.,#5596);
#5589=SURFACE_STYLE_USAGE(.BOTH.,#5597);
#5590=SURFACE_STYLE_USAGE(.BOTH.,#5598);
#5591=SURFACE_STYLE_USAGE(.BOTH.,#5599);
#5592=SURFACE_STYLE_USAGE(.BOTH.,#5600);
#5593=SURFACE_STYLE_USAGE(.BOTH.,#5601);
#5594=SURFACE_STYLE_USAGE(.BOTH.,#5602);
#5595=SURFACE_STYLE_USAGE(.BOTH.,#5603);
#5596=SURFACE_SIDE_STYLE('',(#5604));
#5597=SURFACE_SIDE_STYLE('',(#5605));
#5598=SURFACE_SIDE_STYLE('',(#5606));
#5599=SURFACE_SIDE_STYLE('',(#5607));
#5600=SURFACE_SIDE_STYLE('',(#5608));
#5601=SURFACE_SIDE_STYLE('',(#5609));
#5602=SURFACE_SIDE_STYLE('',(#5610));
#5603=SURFACE_SIDE_STYLE('',(#5611));
#5604=SURFACE_STYLE_FILL_AREA(#5612);
#5605=SURFACE_STYLE_FILL_AREA(#5613);
#5606=SURFACE_STYLE_FILL_AREA(#5614);
#5607=SURFACE_STYLE_FILL_AREA(#5615);
#5608=SURFACE_STYLE_FILL_AREA(#5616);
#5609=SURFACE_STYLE_FILL_AREA(#5617);
#5610=SURFACE_STYLE_FILL_AREA(#5618);
#5611=SURFACE_STYLE_FILL_AREA(#5619);
#5612=FILL_AREA_STYLE('Steel - Satin',(#5620));
#5613=FILL_AREA_STYLE('Opaque(234,234,234)',(#5621));
#5614=FILL_AREA_STYLE('Opaque(196,226,243)',(#5622));
#5615=FILL_AREA_STYLE('Opaque(59,97,180)',(#5623));
#5616=FILL_AREA_STYLE('Opaque(160,160,160)',(#5624));
#5617=FILL_AREA_STYLE('Opaque(248,135,1)',(#5625));
#5618=FILL_AREA_STYLE('Opaque(250,182,1)',(#5626));
#5619=FILL_AREA_STYLE('Opaque(165,165,165)',(#5627));
#5620=FILL_AREA_STYLE_COLOUR('Steel - Satin',#5628);
#5621=FILL_AREA_STYLE_COLOUR('Opaque(234,234,234)',#5629);
#5622=FILL_AREA_STYLE_COLOUR('Opaque(196,226,243)',#5630);
#5623=FILL_AREA_STYLE_COLOUR('Opaque(59,97,180)',#5631);
#5624=FILL_AREA_STYLE_COLOUR('Opaque(160,160,160)',#5632);
#5625=FILL_AREA_STYLE_COLOUR('Opaque(248,135,1)',#5633);
#5626=FILL_AREA_STYLE_COLOUR('Opaque(250,182,1)',#5634);
#5627=FILL_AREA_STYLE_COLOUR('Opaque(165,165,165)',#5635);
#5628=COLOUR_RGB('Steel - Satin', 0.09019608, 0.27058824, 0.51372549);
#5629=COLOUR_RGB('Opaque(234,234,234)', 0.09019608, 0.27058824, 0.51372549);
#5630=COLOUR_RGB('Opaque(196,226,243)', 0.66274510, 0.83137255, 0.94901961);
#5631=COLOUR_RGB('Opaque(59,97,180)', 0.31764706, 0.68627451, 0.89019608);
#5632=COLOUR_RGB('Opaque(160,160,160)', 0.40784314, 0.44705882, 0.49803922);
#5633=COLOUR_RGB('Opaque(248,135,1)', 0.72549020, 0.75294118, 0.79215686);
#5634=COLOUR_RGB('Opaque(250,182,1)', 0.08235294, 0.09019608, 0.10196078);
#5635=COLOUR_RGB('Opaque(165,165,165)', 0.09019608, 0.27058824, 0.51372549);
ENDSEC;
END-ISO-10303-21;
